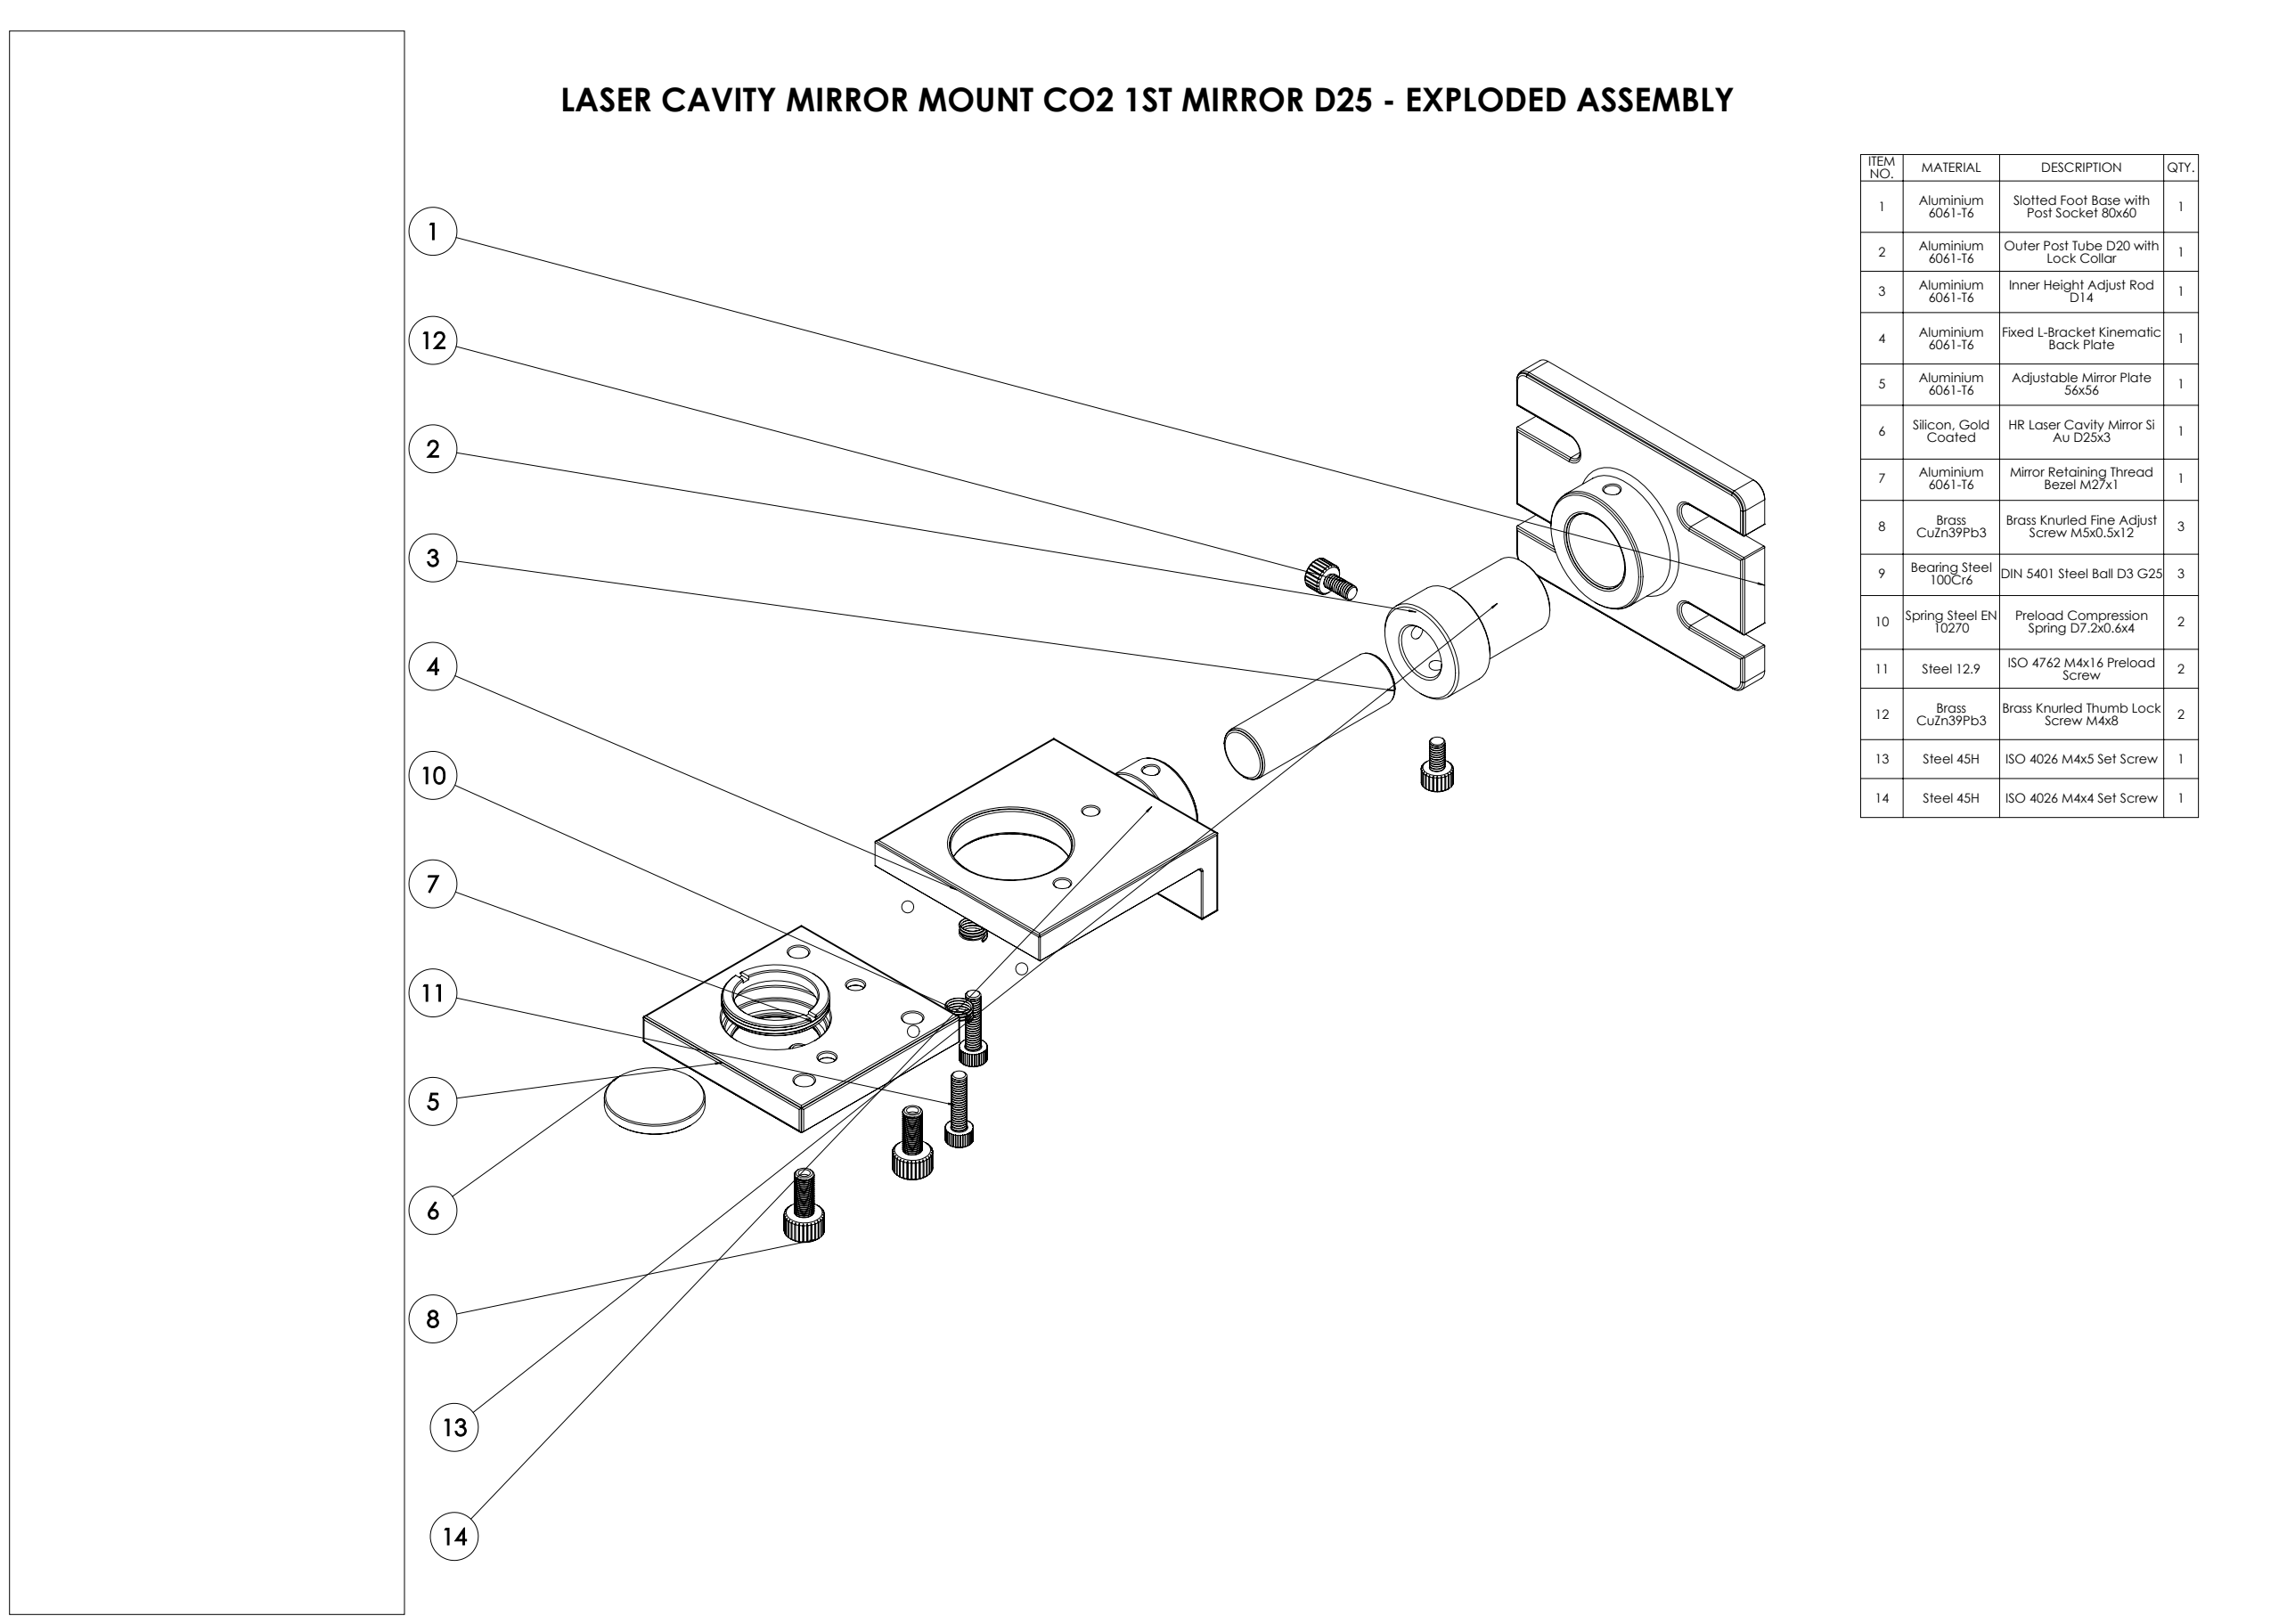
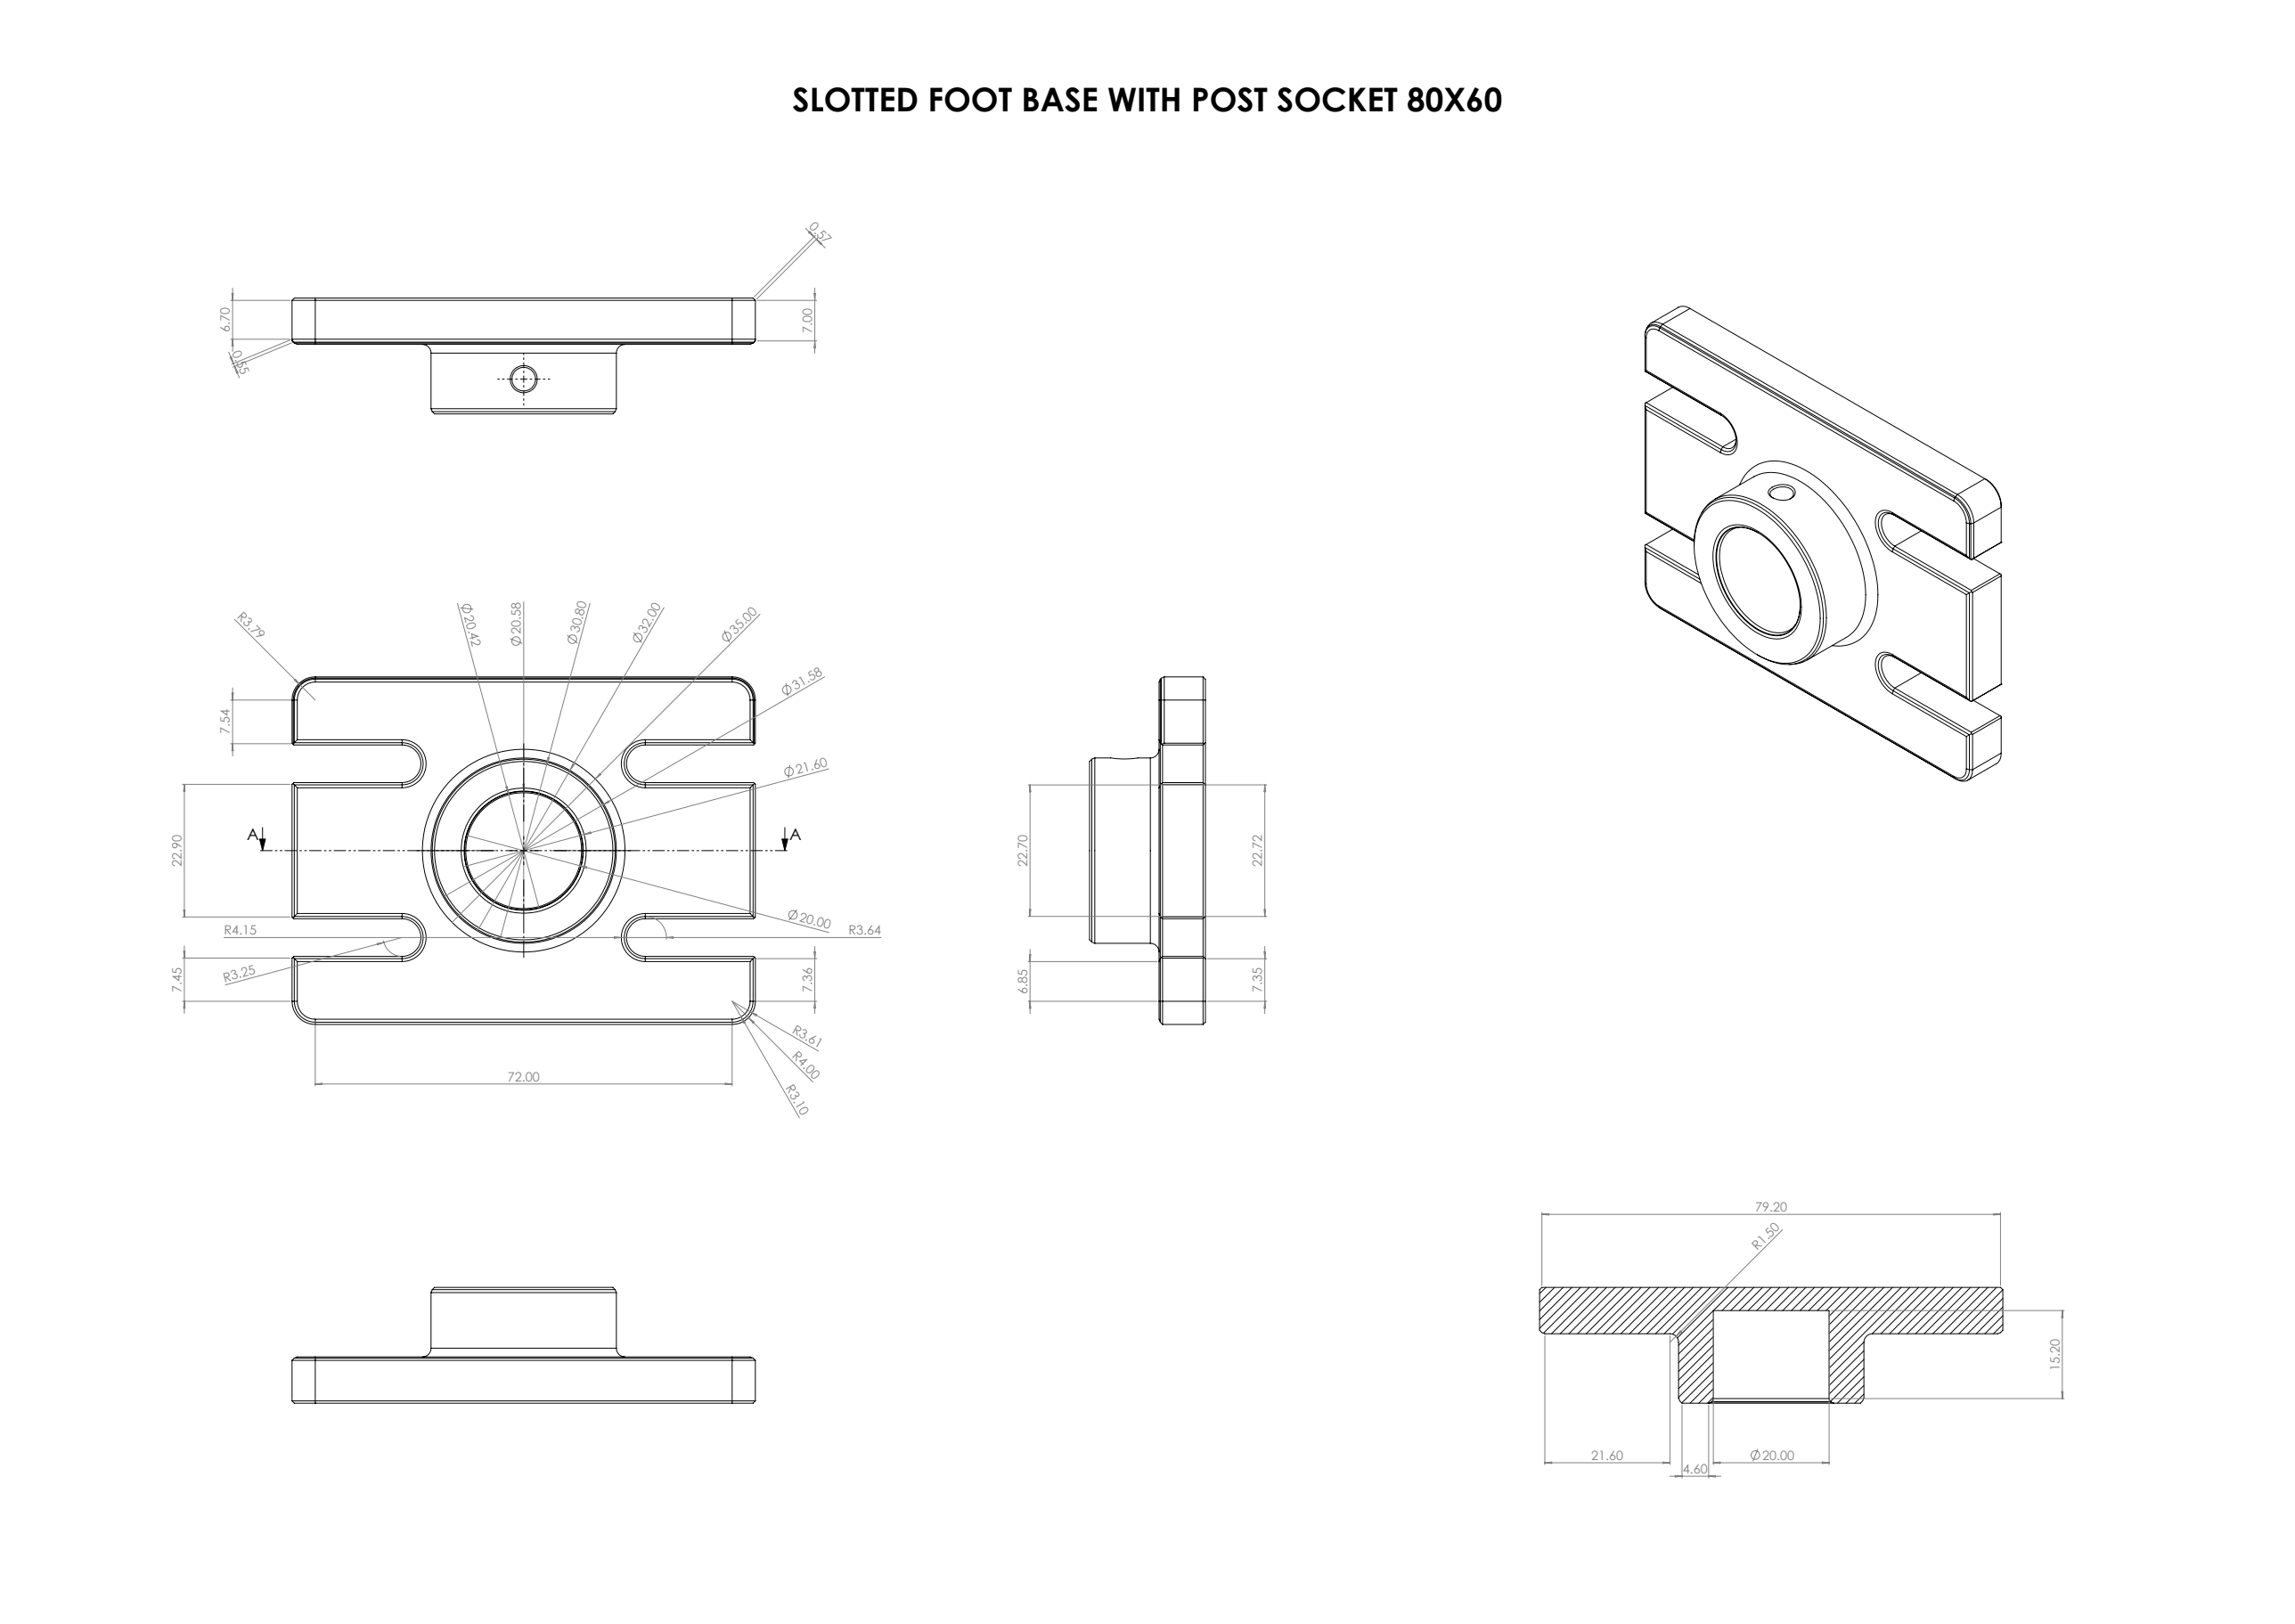
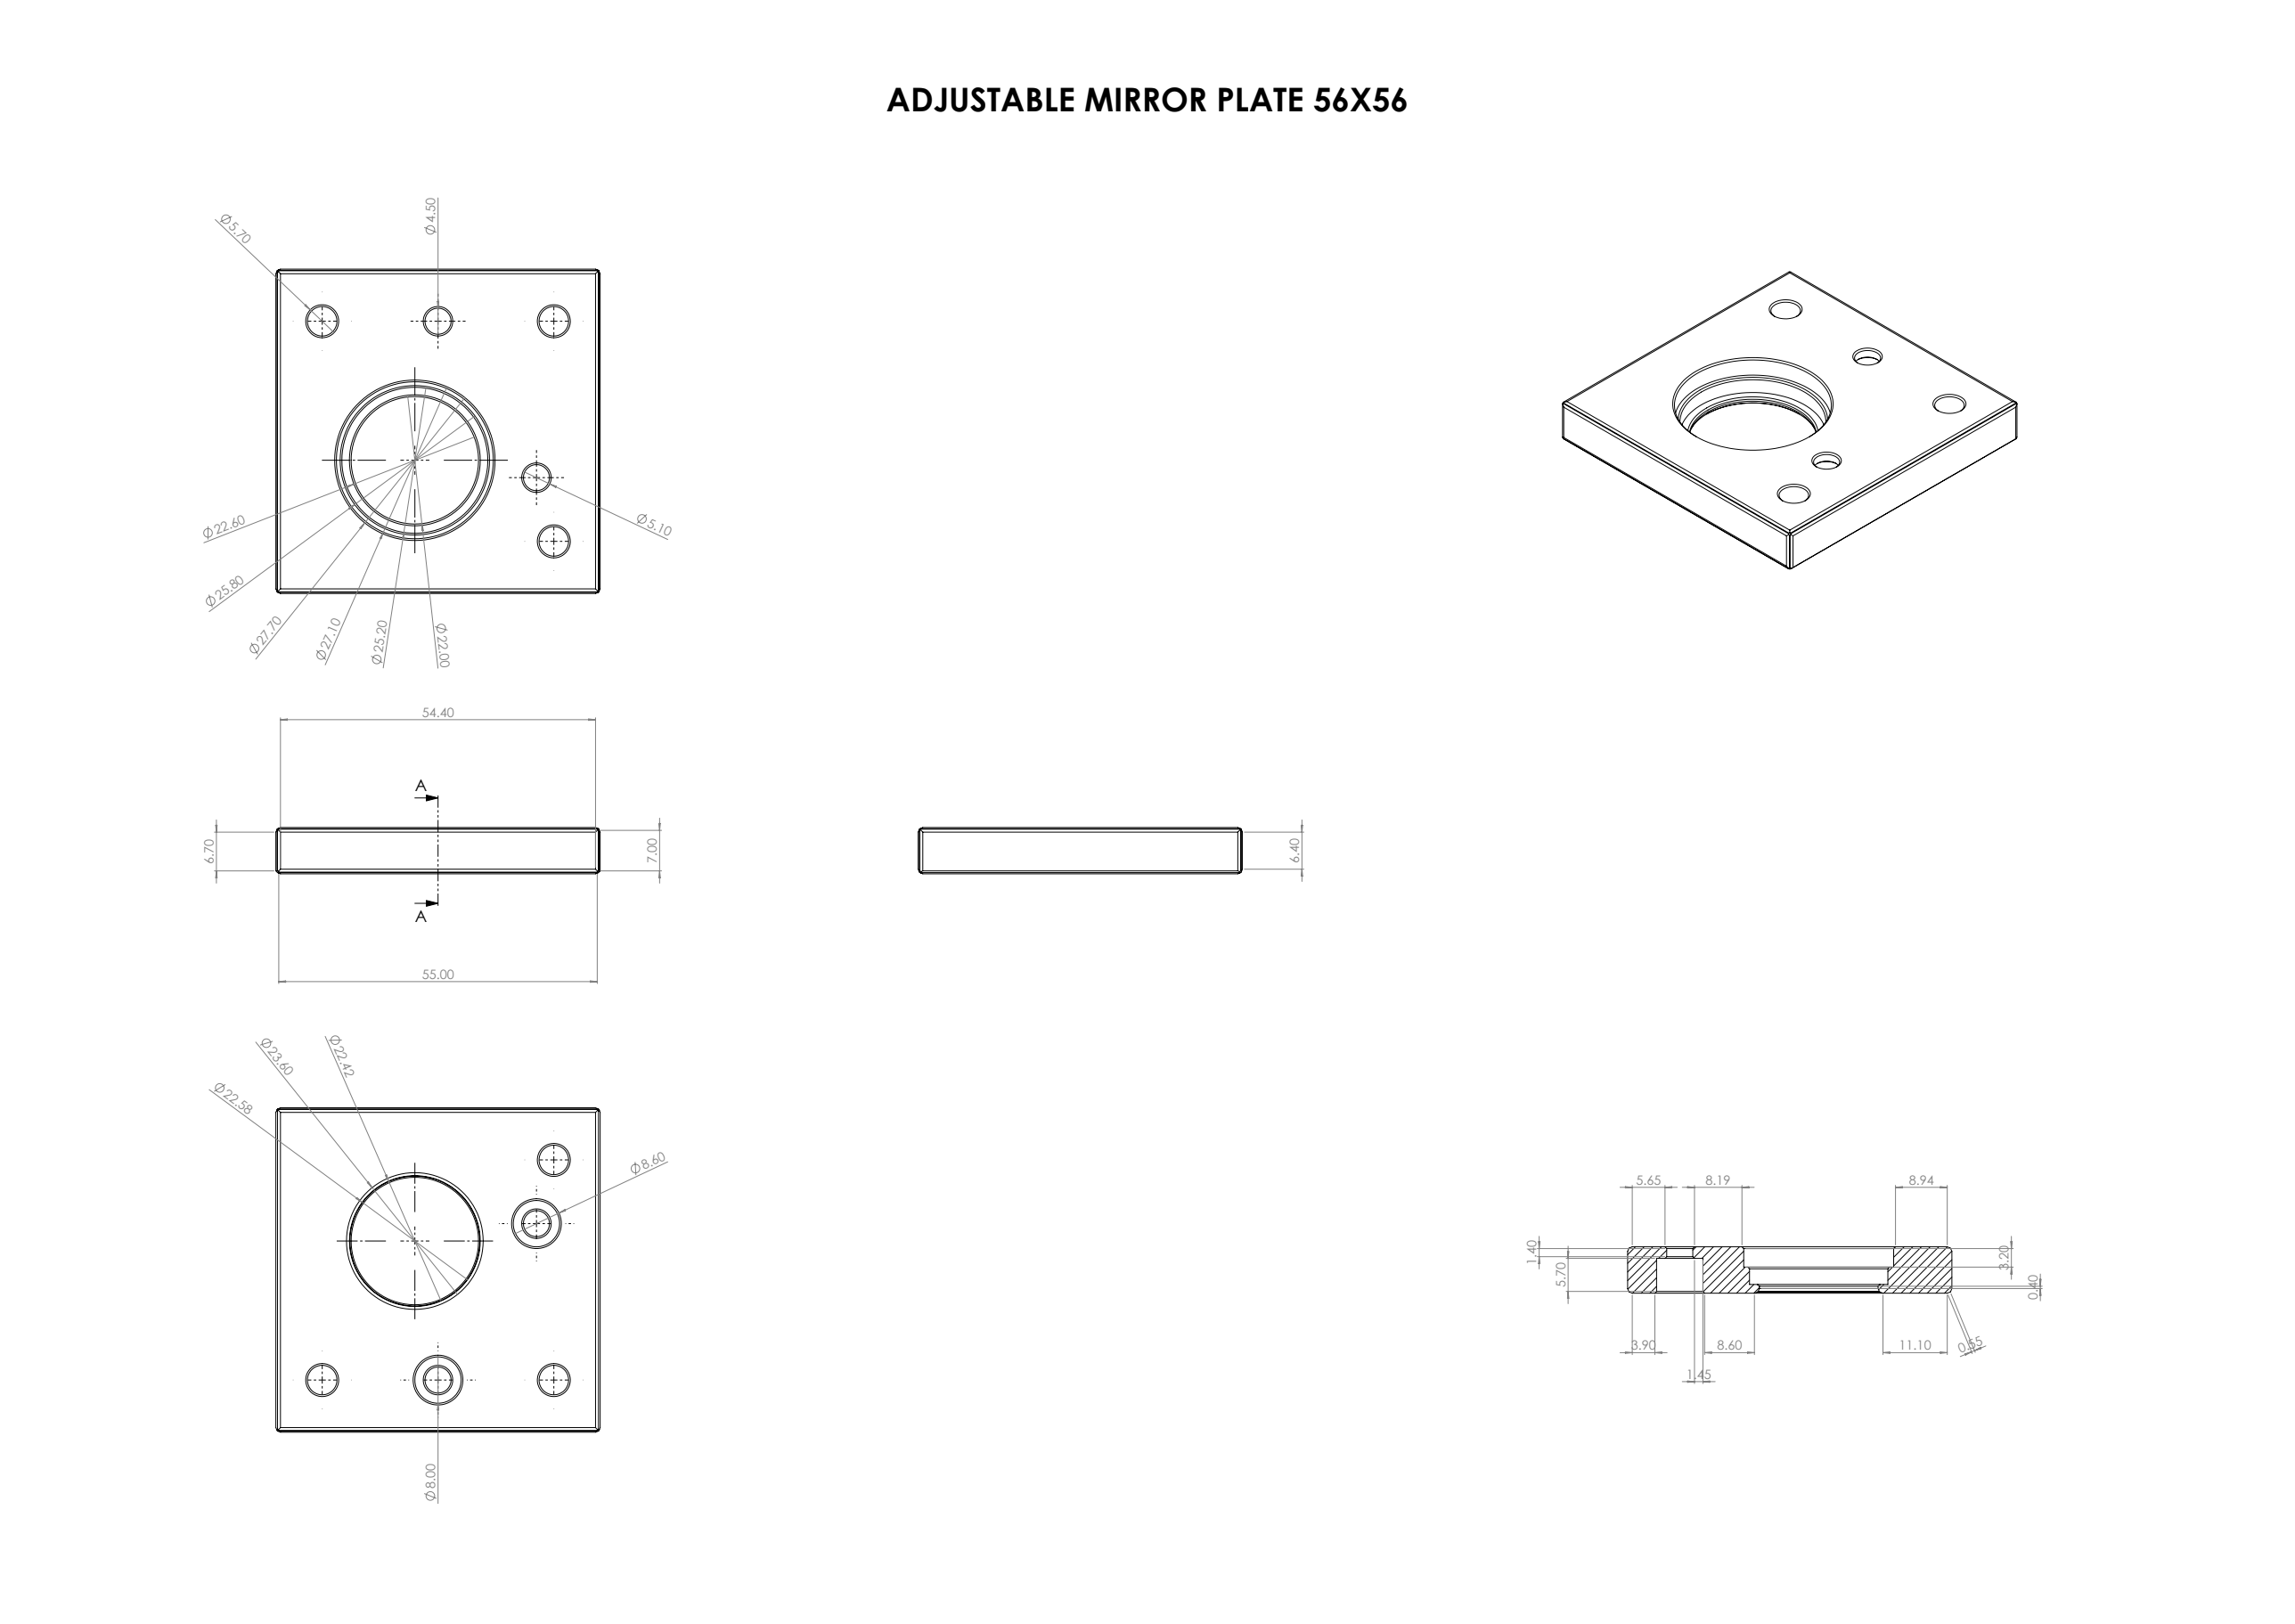
ISO-10303-21;
HEADER;
/* Generated by software containing ST-Developer
 * from STEP Tools, Inc. (www.steptools.com) 
 */

FILE_DESCRIPTION(
/* description */ (''),
/* implementation_level */ '2;1');

FILE_NAME(
/* name */ 
'MAS-303',
/* time_stamp */ '2026-10-20T10:06:23-07:00',
/* author */ (''),
/* organization */ (''),
/* preprocessor_version */ 'ST-DEVELOPER v20.2',
/* originating_system */ 'Autodesk Translation Framework v15.15.0.0',
/* authorisation */ '');

FILE_SCHEMA (('AUTOMOTIVE_DESIGN { 1 0 10303 214 3 1 1 }'));
ENDSEC;

DATA;
#10=MECHANICAL_DESIGN_GEOMETRIC_PRESENTATION_REPRESENTATION('',(#460,#461,
#462,#463,#464,#465,#466,#467,#468,#469,#470,#471,#472,#473),#38611);
#11=ITEM_DEFINED_TRANSFORMATION($,$,#16404,#17784);
#12=ITEM_DEFINED_TRANSFORMATION($,$,#16581,#17785);
#13=ITEM_DEFINED_TRANSFORMATION($,$,#16625,#17786);
#14=ITEM_DEFINED_TRANSFORMATION($,$,#16649,#17787);
#15=ITEM_DEFINED_TRANSFORMATION($,$,#16774,#17788);
#16=ITEM_DEFINED_TRANSFORMATION($,$,#16784,#17789);
#17=ITEM_DEFINED_TRANSFORMATION($,$,#17098,#17790);
#18=ITEM_DEFINED_TRANSFORMATION($,$,#17324,#17791);
#19=ITEM_DEFINED_TRANSFORMATION($,$,#17327,#17792);
#20=ITEM_DEFINED_TRANSFORMATION($,$,#17332,#17793);
#21=ITEM_DEFINED_TRANSFORMATION($,$,#17623,#17794);
#22=ITEM_DEFINED_TRANSFORMATION($,$,#16834,#17795);
#23=ITEM_DEFINED_TRANSFORMATION($,$,#16909,#17796);
#24=ITEM_DEFINED_TRANSFORMATION($,$,#16983,#17797);
#25=ITEM_DEFINED_TRANSFORMATION($,$,#17098,#17798);
#26=ITEM_DEFINED_TRANSFORMATION($,$,#17098,#17799);
#27=ITEM_DEFINED_TRANSFORMATION($,$,#17324,#17800);
#28=ITEM_DEFINED_TRANSFORMATION($,$,#17324,#17801);
#29=ITEM_DEFINED_TRANSFORMATION($,$,#17327,#17802);
#30=ITEM_DEFINED_TRANSFORMATION($,$,#17332,#17803);
#31=ITEM_DEFINED_TRANSFORMATION($,$,#17623,#17804);
#32=(
REPRESENTATION_RELATIONSHIP($,$,#38668,#38667)
REPRESENTATION_RELATIONSHIP_WITH_TRANSFORMATION(#11)
SHAPE_REPRESENTATION_RELATIONSHIP()
);
#33=(
REPRESENTATION_RELATIONSHIP($,$,#38669,#38667)
REPRESENTATION_RELATIONSHIP_WITH_TRANSFORMATION(#12)
SHAPE_REPRESENTATION_RELATIONSHIP()
);
#34=(
REPRESENTATION_RELATIONSHIP($,$,#38670,#38667)
REPRESENTATION_RELATIONSHIP_WITH_TRANSFORMATION(#13)
SHAPE_REPRESENTATION_RELATIONSHIP()
);
#35=(
REPRESENTATION_RELATIONSHIP($,$,#38671,#38667)
REPRESENTATION_RELATIONSHIP_WITH_TRANSFORMATION(#14)
SHAPE_REPRESENTATION_RELATIONSHIP()
);
#36=(
REPRESENTATION_RELATIONSHIP($,$,#38672,#38667)
REPRESENTATION_RELATIONSHIP_WITH_TRANSFORMATION(#15)
SHAPE_REPRESENTATION_RELATIONSHIP()
);
#37=(
REPRESENTATION_RELATIONSHIP($,$,#38673,#38667)
REPRESENTATION_RELATIONSHIP_WITH_TRANSFORMATION(#16)
SHAPE_REPRESENTATION_RELATIONSHIP()
);
#38=(
REPRESENTATION_RELATIONSHIP($,$,#38677,#38667)
REPRESENTATION_RELATIONSHIP_WITH_TRANSFORMATION(#17)
SHAPE_REPRESENTATION_RELATIONSHIP()
);
#39=(
REPRESENTATION_RELATIONSHIP($,$,#38678,#38667)
REPRESENTATION_RELATIONSHIP_WITH_TRANSFORMATION(#18)
SHAPE_REPRESENTATION_RELATIONSHIP()
);
#40=(
REPRESENTATION_RELATIONSHIP($,$,#38679,#38667)
REPRESENTATION_RELATIONSHIP_WITH_TRANSFORMATION(#19)
SHAPE_REPRESENTATION_RELATIONSHIP()
);
#41=(
REPRESENTATION_RELATIONSHIP($,$,#38680,#38667)
REPRESENTATION_RELATIONSHIP_WITH_TRANSFORMATION(#20)
SHAPE_REPRESENTATION_RELATIONSHIP()
);
#42=(
REPRESENTATION_RELATIONSHIP($,$,#38681,#38667)
REPRESENTATION_RELATIONSHIP_WITH_TRANSFORMATION(#21)
SHAPE_REPRESENTATION_RELATIONSHIP()
);
#43=(
REPRESENTATION_RELATIONSHIP($,$,#38674,#38667)
REPRESENTATION_RELATIONSHIP_WITH_TRANSFORMATION(#22)
SHAPE_REPRESENTATION_RELATIONSHIP()
);
#44=(
REPRESENTATION_RELATIONSHIP($,$,#38675,#38667)
REPRESENTATION_RELATIONSHIP_WITH_TRANSFORMATION(#23)
SHAPE_REPRESENTATION_RELATIONSHIP()
);
#45=(
REPRESENTATION_RELATIONSHIP($,$,#38676,#38667)
REPRESENTATION_RELATIONSHIP_WITH_TRANSFORMATION(#24)
SHAPE_REPRESENTATION_RELATIONSHIP()
);
#46=(
REPRESENTATION_RELATIONSHIP($,$,#38677,#38667)
REPRESENTATION_RELATIONSHIP_WITH_TRANSFORMATION(#25)
SHAPE_REPRESENTATION_RELATIONSHIP()
);
#47=(
REPRESENTATION_RELATIONSHIP($,$,#38677,#38667)
REPRESENTATION_RELATIONSHIP_WITH_TRANSFORMATION(#26)
SHAPE_REPRESENTATION_RELATIONSHIP()
);
#48=(
REPRESENTATION_RELATIONSHIP($,$,#38678,#38667)
REPRESENTATION_RELATIONSHIP_WITH_TRANSFORMATION(#27)
SHAPE_REPRESENTATION_RELATIONSHIP()
);
#49=(
REPRESENTATION_RELATIONSHIP($,$,#38678,#38667)
REPRESENTATION_RELATIONSHIP_WITH_TRANSFORMATION(#28)
SHAPE_REPRESENTATION_RELATIONSHIP()
);
#50=(
REPRESENTATION_RELATIONSHIP($,$,#38679,#38667)
REPRESENTATION_RELATIONSHIP_WITH_TRANSFORMATION(#29)
SHAPE_REPRESENTATION_RELATIONSHIP()
);
#51=(
REPRESENTATION_RELATIONSHIP($,$,#38680,#38667)
REPRESENTATION_RELATIONSHIP_WITH_TRANSFORMATION(#30)
SHAPE_REPRESENTATION_RELATIONSHIP()
);
#52=(
REPRESENTATION_RELATIONSHIP($,$,#38681,#38667)
REPRESENTATION_RELATIONSHIP_WITH_TRANSFORMATION(#31)
SHAPE_REPRESENTATION_RELATIONSHIP()
);
#53=CONTEXT_DEPENDENT_SHAPE_REPRESENTATION(#32,#38646);
#54=CONTEXT_DEPENDENT_SHAPE_REPRESENTATION(#33,#38647);
#55=CONTEXT_DEPENDENT_SHAPE_REPRESENTATION(#34,#38648);
#56=CONTEXT_DEPENDENT_SHAPE_REPRESENTATION(#35,#38649);
#57=CONTEXT_DEPENDENT_SHAPE_REPRESENTATION(#36,#38650);
#58=CONTEXT_DEPENDENT_SHAPE_REPRESENTATION(#37,#38651);
#59=CONTEXT_DEPENDENT_SHAPE_REPRESENTATION(#38,#38652);
#60=CONTEXT_DEPENDENT_SHAPE_REPRESENTATION(#39,#38653);
#61=CONTEXT_DEPENDENT_SHAPE_REPRESENTATION(#40,#38654);
#62=CONTEXT_DEPENDENT_SHAPE_REPRESENTATION(#41,#38655);
#63=CONTEXT_DEPENDENT_SHAPE_REPRESENTATION(#42,#38656);
#64=CONTEXT_DEPENDENT_SHAPE_REPRESENTATION(#43,#38657);
#65=CONTEXT_DEPENDENT_SHAPE_REPRESENTATION(#44,#38658);
#66=CONTEXT_DEPENDENT_SHAPE_REPRESENTATION(#45,#38659);
#67=CONTEXT_DEPENDENT_SHAPE_REPRESENTATION(#46,#38660);
#68=CONTEXT_DEPENDENT_SHAPE_REPRESENTATION(#47,#38661);
#69=CONTEXT_DEPENDENT_SHAPE_REPRESENTATION(#48,#38662);
#70=CONTEXT_DEPENDENT_SHAPE_REPRESENTATION(#49,#38663);
#71=CONTEXT_DEPENDENT_SHAPE_REPRESENTATION(#50,#38664);
#72=CONTEXT_DEPENDENT_SHAPE_REPRESENTATION(#51,#38665);
#73=CONTEXT_DEPENDENT_SHAPE_REPRESENTATION(#52,#38666);
#74=NEXT_ASSEMBLY_USAGE_OCCURRENCE(
'01_Slotted_Foot_Base_with_Post_Socket_80x60:1',
'01_Slotted_Foot_Base_with_Post_Socket_80x60:1',
'01_Slotted_Foot_Base_with_Post_Socket_80x60:1',#38683,#38684,
'01_Slotted_Foot_Base_with_Post_Socket_80x60:1');
#75=NEXT_ASSEMBLY_USAGE_OCCURRENCE(
'02_Outer_Post_Tube_D20_with_Lock_Collar:1',
'02_Outer_Post_Tube_D20_with_Lock_Collar:1',
'02_Outer_Post_Tube_D20_with_Lock_Collar:1',#38683,#38685,
'02_Outer_Post_Tube_D20_with_Lock_Collar:1');
#76=NEXT_ASSEMBLY_USAGE_OCCURRENCE('03_Inner_Height_Adjust_Rod_D14:1',
'03_Inner_Height_Adjust_Rod_D14:1','03_Inner_Height_Adjust_Rod_D14:1',#38683,
#38686,'03_Inner_Height_Adjust_Rod_D14:1');
#77=NEXT_ASSEMBLY_USAGE_OCCURRENCE('05_Adjustable_Mirror_Plate_56x56:1',
'05_Adjustable_Mirror_Plate_56x56:1',
'05_Adjustable_Mirror_Plate_56x56:1',#38683,#38687,
'05_Adjustable_Mirror_Plate_56x56:1');
#78=NEXT_ASSEMBLY_USAGE_OCCURRENCE(
'06_HR_Laser_Cavity_Mirror_Si_Au_D25x3:1',
'06_HR_Laser_Cavity_Mirror_Si_Au_D25x3:1',
'06_HR_Laser_Cavity_Mirror_Si_Au_D25x3:1',#38683,#38688,
'06_HR_Laser_Cavity_Mirror_Si_Au_D25x3:1');
#79=NEXT_ASSEMBLY_USAGE_OCCURRENCE(
'07_Mirror_Retaining_Thread_Bezel_M27x1:1',
'07_Mirror_Retaining_Thread_Bezel_M27x1:1',
'07_Mirror_Retaining_Thread_Bezel_M27x1:1',#38683,#38689,
'07_Mirror_Retaining_Thread_Bezel_M27x1:1');
#80=NEXT_ASSEMBLY_USAGE_OCCURRENCE(
'08_Brass_Knurled_Fine_Adjust_Screw_M5x0.5x12:1',
'08_Brass_Knurled_Fine_Adjust_Screw_M5x0.5x12:1',
'08_Brass_Knurled_Fine_Adjust_Screw_M5x0.5x12:1',#38683,#38693,
'08_Brass_Knurled_Fine_Adjust_Screw_M5x0.5x12:1');
#81=NEXT_ASSEMBLY_USAGE_OCCURRENCE('09_DIN_5401_Steel_Ball_D3_G25:1',
'09_DIN_5401_Steel_Ball_D3_G25:1','09_DIN_5401_Steel_Ball_D3_G25:1',#38683,
#38694,'09_DIN_5401_Steel_Ball_D3_G25:1');
#82=NEXT_ASSEMBLY_USAGE_OCCURRENCE(
'10_Preload_Compression_Spring_D7.2x0.6x4:1',
'10_Preload_Compression_Spring_D7.2x0.6x4:1',
'10_Preload_Compression_Spring_D7.2x0.6x4:1',#38683,#38695,
'10_Preload_Compression_Spring_D7.2x0.6x4:1');
#83=NEXT_ASSEMBLY_USAGE_OCCURRENCE('11_ISO_4762_M4x16_Preload_Screw:1',
'11_ISO_4762_M4x16_Preload_Screw:1','11_ISO_4762_M4x16_Preload_Screw:1',
#38683,#38696,'11_ISO_4762_M4x16_Preload_Screw:1');
#84=NEXT_ASSEMBLY_USAGE_OCCURRENCE(
'12_Brass_Knurled_Thumb_Lock_Screw_M4x8:1',
'12_Brass_Knurled_Thumb_Lock_Screw_M4x8:1',
'12_Brass_Knurled_Thumb_Lock_Screw_M4x8:1',#38683,#38697,
'12_Brass_Knurled_Thumb_Lock_Screw_M4x8:1');
#85=NEXT_ASSEMBLY_USAGE_OCCURRENCE('13_ISO_4026_M4x5_Set_Screw:1',
'13_ISO_4026_M4x5_Set_Screw:1','13_ISO_4026_M4x5_Set_Screw:1',#38683,#38690,
'13_ISO_4026_M4x5_Set_Screw:1');
#86=NEXT_ASSEMBLY_USAGE_OCCURRENCE('14_ISO_4026_M4x4_Set_Screw:1',
'14_ISO_4026_M4x4_Set_Screw:1','14_ISO_4026_M4x4_Set_Screw:1',#38683,#38691,
'14_ISO_4026_M4x4_Set_Screw:1');
#87=NEXT_ASSEMBLY_USAGE_OCCURRENCE(
'04_Fixed_L-Bracket_Kinematic_Back_Plate:1',
'04_Fixed_L-Bracket_Kinematic_Back_Plate:1',
'04_Fixed_L-Bracket_Kinematic_Back_Plate:1',#38683,#38692,
'04_Fixed_L-Bracket_Kinematic_Back_Plate:1');
#88=NEXT_ASSEMBLY_USAGE_OCCURRENCE(
'08_Brass_Knurled_Fine_Adjust_Screw_M5x0.5x12:2',
'08_Brass_Knurled_Fine_Adjust_Screw_M5x0.5x12:2',
'08_Brass_Knurled_Fine_Adjust_Screw_M5x0.5x12:2',#38683,#38693,
'08_Brass_Knurled_Fine_Adjust_Screw_M5x0.5x12:2');
#89=NEXT_ASSEMBLY_USAGE_OCCURRENCE(
'08_Brass_Knurled_Fine_Adjust_Screw_M5x0.5x12:3',
'08_Brass_Knurled_Fine_Adjust_Screw_M5x0.5x12:3',
'08_Brass_Knurled_Fine_Adjust_Screw_M5x0.5x12:3',#38683,#38693,
'08_Brass_Knurled_Fine_Adjust_Screw_M5x0.5x12:3');
#90=NEXT_ASSEMBLY_USAGE_OCCURRENCE('09_DIN_5401_Steel_Ball_D3_G25:2',
'09_DIN_5401_Steel_Ball_D3_G25:2','09_DIN_5401_Steel_Ball_D3_G25:2',#38683,
#38694,'09_DIN_5401_Steel_Ball_D3_G25:2');
#91=NEXT_ASSEMBLY_USAGE_OCCURRENCE('09_DIN_5401_Steel_Ball_D3_G25:3',
'09_DIN_5401_Steel_Ball_D3_G25:3','09_DIN_5401_Steel_Ball_D3_G25:3',#38683,
#38694,'09_DIN_5401_Steel_Ball_D3_G25:3');
#92=NEXT_ASSEMBLY_USAGE_OCCURRENCE(
'10_Preload_Compression_Spring_D7.2x0.6x4:2',
'10_Preload_Compression_Spring_D7.2x0.6x4:2',
'10_Preload_Compression_Spring_D7.2x0.6x4:2',#38683,#38695,
'10_Preload_Compression_Spring_D7.2x0.6x4:2');
#93=NEXT_ASSEMBLY_USAGE_OCCURRENCE('11_ISO_4762_M4x16_Preload_Screw:2',
'11_ISO_4762_M4x16_Preload_Screw:2','11_ISO_4762_M4x16_Preload_Screw:2',
#38683,#38696,'11_ISO_4762_M4x16_Preload_Screw:2');
#94=NEXT_ASSEMBLY_USAGE_OCCURRENCE(
'12_Brass_Knurled_Thumb_Lock_Screw_M4x8:2',
'12_Brass_Knurled_Thumb_Lock_Screw_M4x8:2',
'12_Brass_Knurled_Thumb_Lock_Screw_M4x8:2',#38683,#38697,
'12_Brass_Knurled_Thumb_Lock_Screw_M4x8:2');
#95=SPHERICAL_SURFACE('',#17325,0.15);
#96=ELLIPSE('',#16996,1.69705627484771,1.2);
#97=ELLIPSE('',#16998,1.69705627484771,1.2);
#98=(
BOUNDED_CURVE()
B_SPLINE_CURVE(2,(#24495,#24496,#24497),.UNSPECIFIED.,.F.,.F.)
B_SPLINE_CURVE_WITH_KNOTS((3,3),(0.,0.048540461555457),.UNSPECIFIED.)
CURVE()
GEOMETRIC_REPRESENTATION_ITEM()
RATIONAL_B_SPLINE_CURVE((1.,1.0000974490119,1.00002789674321))
REPRESENTATION_ITEM('')
);
#99=(
BOUNDED_CURVE()
B_SPLINE_CURVE(2,(#24501,#24502,#24503),.UNSPECIFIED.,.F.,.F.)
B_SPLINE_CURVE_WITH_KNOTS((3,3),(0.,0.0425206671334367),.UNSPECIFIED.)
CURVE()
GEOMETRIC_REPRESENTATION_ITEM()
RATIONAL_B_SPLINE_CURVE((1.,1.00010008479633,1.))
REPRESENTATION_ITEM('')
);
#100=(
BOUNDED_CURVE()
B_SPLINE_CURVE(2,(#24513,#24514,#24515),.UNSPECIFIED.,.F.,.F.)
B_SPLINE_CURVE_WITH_KNOTS((3,3),(0.,0.0425206671334366),.UNSPECIFIED.)
CURVE()
GEOMETRIC_REPRESENTATION_ITEM()
RATIONAL_B_SPLINE_CURVE((1.,1.00010008445539,1.))
REPRESENTATION_ITEM('')
);
#101=(
BOUNDED_CURVE()
B_SPLINE_CURVE(2,(#24518,#24519,#24520),.UNSPECIFIED.,.F.,.F.)
B_SPLINE_CURVE_WITH_KNOTS((3,3),(0.00810844555795414,0.0566489071109945),
 .UNSPECIFIED.)
CURVE()
GEOMETRIC_REPRESENTATION_ITEM()
RATIONAL_B_SPLINE_CURVE((1.00002789660287,1.00009744852162,1.))
REPRESENTATION_ITEM('')
);
#102=(
BOUNDED_CURVE()
B_SPLINE_CURVE(2,(#24534,#24535,#24536),.UNSPECIFIED.,.F.,.F.)
B_SPLINE_CURVE_WITH_KNOTS((3,3),(0.,0.0485404615530411),.UNSPECIFIED.)
CURVE()
GEOMETRIC_REPRESENTATION_ITEM()
RATIONAL_B_SPLINE_CURVE((1.,1.00009744852162,1.00002789660287))
REPRESENTATION_ITEM('')
);
#103=(
BOUNDED_CURVE()
B_SPLINE_CURVE(2,(#24540,#24541,#24542),.UNSPECIFIED.,.F.,.F.)
B_SPLINE_CURVE_WITH_KNOTS((3,3),(0.,0.0425206671334366),.UNSPECIFIED.)
CURVE()
GEOMETRIC_REPRESENTATION_ITEM()
RATIONAL_B_SPLINE_CURVE((1.,1.00010008445539,1.))
REPRESENTATION_ITEM('')
);
#104=(
BOUNDED_CURVE()
B_SPLINE_CURVE(2,(#24552,#24553,#24554),.UNSPECIFIED.,.F.,.F.)
B_SPLINE_CURVE_WITH_KNOTS((3,3),(0.,0.0425206671334367),.UNSPECIFIED.)
CURVE()
GEOMETRIC_REPRESENTATION_ITEM()
RATIONAL_B_SPLINE_CURVE((1.,1.00010008479633,1.))
REPRESENTATION_ITEM('')
);
#105=(
BOUNDED_CURVE()
B_SPLINE_CURVE(2,(#24557,#24558,#24559),.UNSPECIFIED.,.F.,.F.)
B_SPLINE_CURVE_WITH_KNOTS((3,3),(0.00810844555553747,0.0566489071109946),
 .UNSPECIFIED.)
CURVE()
GEOMETRIC_REPRESENTATION_ITEM()
RATIONAL_B_SPLINE_CURVE((1.00002789674321,1.0000974490119,1.))
REPRESENTATION_ITEM('')
);
#106=(
BOUNDED_CURVE()
B_SPLINE_CURVE(2,(#25662,#25663,#25664),.UNSPECIFIED.,.F.,.F.)
B_SPLINE_CURVE_WITH_KNOTS((3,3),(0.,0.00350597452849922),.UNSPECIFIED.)
CURVE()
GEOMETRIC_REPRESENTATION_ITEM()
RATIONAL_B_SPLINE_CURVE((1.,1.00010739978215,1.))
REPRESENTATION_ITEM('')
);
#107=(
BOUNDED_CURVE()
B_SPLINE_CURVE(2,(#25666,#25667,#25668),.UNSPECIFIED.,.F.,.F.)
B_SPLINE_CURVE_WITH_KNOTS((3,3),(0.,0.00350597452849927),.UNSPECIFIED.)
CURVE()
GEOMETRIC_REPRESENTATION_ITEM()
RATIONAL_B_SPLINE_CURVE((1.,1.00010739978482,1.))
REPRESENTATION_ITEM('')
);
#108=(
BOUNDED_CURVE()
B_SPLINE_CURVE(2,(#25671,#25672,#25673),.UNSPECIFIED.,.F.,.F.)
B_SPLINE_CURVE_WITH_KNOTS((3,3),(0.,0.0035059745284993),.UNSPECIFIED.)
CURVE()
GEOMETRIC_REPRESENTATION_ITEM()
RATIONAL_B_SPLINE_CURVE((1.,1.00010739978303,1.))
REPRESENTATION_ITEM('')
);
#109=(
BOUNDED_CURVE()
B_SPLINE_CURVE(2,(#25675,#25676,#25677),.UNSPECIFIED.,.F.,.F.)
B_SPLINE_CURVE_WITH_KNOTS((3,3),(0.,0.00350597452849931),.UNSPECIFIED.)
CURVE()
GEOMETRIC_REPRESENTATION_ITEM()
RATIONAL_B_SPLINE_CURVE((1.,1.00010739978394,1.))
REPRESENTATION_ITEM('')
);
#110=(
BOUNDED_CURVE()
B_SPLINE_CURVE(2,(#25680,#25681,#25682),.UNSPECIFIED.,.F.,.F.)
B_SPLINE_CURVE_WITH_KNOTS((3,3),(0.,0.0035059745284993),.UNSPECIFIED.)
CURVE()
GEOMETRIC_REPRESENTATION_ITEM()
RATIONAL_B_SPLINE_CURVE((1.,1.00010739978631,1.))
REPRESENTATION_ITEM('')
);
#111=(
BOUNDED_CURVE()
B_SPLINE_CURVE(2,(#25684,#25685,#25686),.UNSPECIFIED.,.F.,.F.)
B_SPLINE_CURVE_WITH_KNOTS((3,3),(0.,0.00350597452849929),.UNSPECIFIED.)
CURVE()
GEOMETRIC_REPRESENTATION_ITEM()
RATIONAL_B_SPLINE_CURVE((1.,1.00010739978645,1.))
REPRESENTATION_ITEM('')
);
#112=(
BOUNDED_CURVE()
B_SPLINE_CURVE(2,(#25689,#25690,#25691),.UNSPECIFIED.,.F.,.F.)
B_SPLINE_CURVE_WITH_KNOTS((3,3),(0.,0.0035059745284993),.UNSPECIFIED.)
CURVE()
GEOMETRIC_REPRESENTATION_ITEM()
RATIONAL_B_SPLINE_CURVE((1.,1.00010739979569,1.))
REPRESENTATION_ITEM('')
);
#113=(
BOUNDED_CURVE()
B_SPLINE_CURVE(2,(#25693,#25694,#25695),.UNSPECIFIED.,.F.,.F.)
B_SPLINE_CURVE_WITH_KNOTS((3,3),(0.,0.0035059745284993),.UNSPECIFIED.)
CURVE()
GEOMETRIC_REPRESENTATION_ITEM()
RATIONAL_B_SPLINE_CURVE((1.,1.00010739979698,1.))
REPRESENTATION_ITEM('')
);
#114=(
BOUNDED_CURVE()
B_SPLINE_CURVE(2,(#25698,#25699,#25700),.UNSPECIFIED.,.F.,.F.)
B_SPLINE_CURVE_WITH_KNOTS((3,3),(0.,0.00350597452849928),.UNSPECIFIED.)
CURVE()
GEOMETRIC_REPRESENTATION_ITEM()
RATIONAL_B_SPLINE_CURVE((1.,1.00010739978256,1.))
REPRESENTATION_ITEM('')
);
#115=(
BOUNDED_CURVE()
B_SPLINE_CURVE(2,(#25702,#25703,#25704),.UNSPECIFIED.,.F.,.F.)
B_SPLINE_CURVE_WITH_KNOTS((3,3),(0.,0.00350597452849928),.UNSPECIFIED.)
CURVE()
GEOMETRIC_REPRESENTATION_ITEM()
RATIONAL_B_SPLINE_CURVE((1.,1.00010739978752,1.))
REPRESENTATION_ITEM('')
);
#116=(
BOUNDED_CURVE()
B_SPLINE_CURVE(2,(#25707,#25708,#25709),.UNSPECIFIED.,.F.,.F.)
B_SPLINE_CURVE_WITH_KNOTS((3,3),(0.,0.0035059745284993),.UNSPECIFIED.)
CURVE()
GEOMETRIC_REPRESENTATION_ITEM()
RATIONAL_B_SPLINE_CURVE((1.,1.0001073997843,1.))
REPRESENTATION_ITEM('')
);
#117=(
BOUNDED_CURVE()
B_SPLINE_CURVE(2,(#25711,#25712,#25713),.UNSPECIFIED.,.F.,.F.)
B_SPLINE_CURVE_WITH_KNOTS((3,3),(0.,0.00350597452849929),.UNSPECIFIED.)
CURVE()
GEOMETRIC_REPRESENTATION_ITEM()
RATIONAL_B_SPLINE_CURVE((1.,1.00010739978875,1.))
REPRESENTATION_ITEM('')
);
#118=(
BOUNDED_CURVE()
B_SPLINE_CURVE(2,(#26703,#26704,#26705),.UNSPECIFIED.,.F.,.F.)
B_SPLINE_CURVE_WITH_KNOTS((3,3),(0.,0.00350597452849922),.UNSPECIFIED.)
CURVE()
GEOMETRIC_REPRESENTATION_ITEM()
RATIONAL_B_SPLINE_CURVE((1.,1.00010739978215,1.))
REPRESENTATION_ITEM('')
);
#119=(
BOUNDED_CURVE()
B_SPLINE_CURVE(2,(#26707,#26708,#26709),.UNSPECIFIED.,.F.,.F.)
B_SPLINE_CURVE_WITH_KNOTS((3,3),(0.,0.00350597452849927),.UNSPECIFIED.)
CURVE()
GEOMETRIC_REPRESENTATION_ITEM()
RATIONAL_B_SPLINE_CURVE((1.,1.00010739978482,1.))
REPRESENTATION_ITEM('')
);
#120=(
BOUNDED_CURVE()
B_SPLINE_CURVE(2,(#26712,#26713,#26714),.UNSPECIFIED.,.F.,.F.)
B_SPLINE_CURVE_WITH_KNOTS((3,3),(0.,0.0035059745284993),.UNSPECIFIED.)
CURVE()
GEOMETRIC_REPRESENTATION_ITEM()
RATIONAL_B_SPLINE_CURVE((1.,1.00010739978303,1.))
REPRESENTATION_ITEM('')
);
#121=(
BOUNDED_CURVE()
B_SPLINE_CURVE(2,(#26716,#26717,#26718),.UNSPECIFIED.,.F.,.F.)
B_SPLINE_CURVE_WITH_KNOTS((3,3),(0.,0.00350597452849931),.UNSPECIFIED.)
CURVE()
GEOMETRIC_REPRESENTATION_ITEM()
RATIONAL_B_SPLINE_CURVE((1.,1.00010739978394,1.))
REPRESENTATION_ITEM('')
);
#122=(
BOUNDED_CURVE()
B_SPLINE_CURVE(2,(#26721,#26722,#26723),.UNSPECIFIED.,.F.,.F.)
B_SPLINE_CURVE_WITH_KNOTS((3,3),(0.,0.0035059745284993),.UNSPECIFIED.)
CURVE()
GEOMETRIC_REPRESENTATION_ITEM()
RATIONAL_B_SPLINE_CURVE((1.,1.00010739978631,1.))
REPRESENTATION_ITEM('')
);
#123=(
BOUNDED_CURVE()
B_SPLINE_CURVE(2,(#26725,#26726,#26727),.UNSPECIFIED.,.F.,.F.)
B_SPLINE_CURVE_WITH_KNOTS((3,3),(0.,0.00350597452849929),.UNSPECIFIED.)
CURVE()
GEOMETRIC_REPRESENTATION_ITEM()
RATIONAL_B_SPLINE_CURVE((1.,1.00010739978645,1.))
REPRESENTATION_ITEM('')
);
#124=(
BOUNDED_CURVE()
B_SPLINE_CURVE(2,(#26730,#26731,#26732),.UNSPECIFIED.,.F.,.F.)
B_SPLINE_CURVE_WITH_KNOTS((3,3),(0.,0.0035059745284993),.UNSPECIFIED.)
CURVE()
GEOMETRIC_REPRESENTATION_ITEM()
RATIONAL_B_SPLINE_CURVE((1.,1.00010739979569,1.))
REPRESENTATION_ITEM('')
);
#125=(
BOUNDED_CURVE()
B_SPLINE_CURVE(2,(#26734,#26735,#26736),.UNSPECIFIED.,.F.,.F.)
B_SPLINE_CURVE_WITH_KNOTS((3,3),(0.,0.0035059745284993),.UNSPECIFIED.)
CURVE()
GEOMETRIC_REPRESENTATION_ITEM()
RATIONAL_B_SPLINE_CURVE((1.,1.00010739979698,1.))
REPRESENTATION_ITEM('')
);
#126=(
BOUNDED_CURVE()
B_SPLINE_CURVE(2,(#26739,#26740,#26741),.UNSPECIFIED.,.F.,.F.)
B_SPLINE_CURVE_WITH_KNOTS((3,3),(0.,0.00350597452849928),.UNSPECIFIED.)
CURVE()
GEOMETRIC_REPRESENTATION_ITEM()
RATIONAL_B_SPLINE_CURVE((1.,1.00010739978256,1.))
REPRESENTATION_ITEM('')
);
#127=(
BOUNDED_CURVE()
B_SPLINE_CURVE(2,(#26743,#26744,#26745),.UNSPECIFIED.,.F.,.F.)
B_SPLINE_CURVE_WITH_KNOTS((3,3),(0.,0.00350597452849928),.UNSPECIFIED.)
CURVE()
GEOMETRIC_REPRESENTATION_ITEM()
RATIONAL_B_SPLINE_CURVE((1.,1.00010739978752,1.))
REPRESENTATION_ITEM('')
);
#128=(
BOUNDED_CURVE()
B_SPLINE_CURVE(2,(#26748,#26749,#26750),.UNSPECIFIED.,.F.,.F.)
B_SPLINE_CURVE_WITH_KNOTS((3,3),(0.,0.0035059745284993),.UNSPECIFIED.)
CURVE()
GEOMETRIC_REPRESENTATION_ITEM()
RATIONAL_B_SPLINE_CURVE((1.,1.0001073997843,1.))
REPRESENTATION_ITEM('')
);
#129=(
BOUNDED_CURVE()
B_SPLINE_CURVE(2,(#26752,#26753,#26754),.UNSPECIFIED.,.F.,.F.)
B_SPLINE_CURVE_WITH_KNOTS((3,3),(0.,0.00350597452849929),.UNSPECIFIED.)
CURVE()
GEOMETRIC_REPRESENTATION_ITEM()
RATIONAL_B_SPLINE_CURVE((1.,1.00010739978875,1.))
REPRESENTATION_ITEM('')
);
#130=(
BOUNDED_CURVE()
B_SPLINE_CURVE(2,(#27130,#27131,#27132),.UNSPECIFIED.,.F.,.F.)
B_SPLINE_CURVE_WITH_KNOTS((3,3),(0.245470547469808,0.342025381879347),
 .UNSPECIFIED.)
CURVE()
GEOMETRIC_REPRESENTATION_ITEM()
RATIONAL_B_SPLINE_CURVE((1.,1.,1.))
REPRESENTATION_ITEM('')
);
#131=(
BOUNDED_CURVE()
B_SPLINE_CURVE(2,(#27135,#27136,#27137),.UNSPECIFIED.,.F.,.F.)
B_SPLINE_CURVE_WITH_KNOTS((3,3),(0.165943124807515,0.262497959217054),
 .UNSPECIFIED.)
CURVE()
GEOMETRIC_REPRESENTATION_ITEM()
RATIONAL_B_SPLINE_CURVE((1.,1.,1.))
REPRESENTATION_ITEM('')
);
#132=(
BOUNDED_CURVE()
B_SPLINE_CURVE(2,(#30814,#30815,#30816),.UNSPECIFIED.,.F.,.F.)
B_SPLINE_CURVE_WITH_KNOTS((3,3),(0.0467199500563867,0.0898699663113549),
 .UNSPECIFIED.)
CURVE()
GEOMETRIC_REPRESENTATION_ITEM()
RATIONAL_B_SPLINE_CURVE((1.00126937543075,1.00122087809448,1.))
REPRESENTATION_ITEM('')
);
#133=(
BOUNDED_CURVE()
B_SPLINE_CURVE(2,(#30820,#30821,#30822),.UNSPECIFIED.,.F.,.F.)
B_SPLINE_CURVE_WITH_KNOTS((3,3),(0.,0.0436887632258073),.UNSPECIFIED.)
CURVE()
GEOMETRIC_REPRESENTATION_ITEM()
RATIONAL_B_SPLINE_CURVE((1.,1.00100330533763,1.00083425612165))
REPRESENTATION_ITEM('')
);
#134=(
BOUNDED_CURVE()
B_SPLINE_CURVE(2,(#30826,#30827,#30828),.UNSPECIFIED.,.F.,.F.)
B_SPLINE_CURVE_WITH_KNOTS((3,3),(0.,0.0431500162549626),.UNSPECIFIED.)
CURVE()
GEOMETRIC_REPRESENTATION_ITEM()
RATIONAL_B_SPLINE_CURVE((1.,1.00122087809439,1.00126937543066))
REPRESENTATION_ITEM('')
);
#135=(
BOUNDED_CURVE()
B_SPLINE_CURVE(2,(#30831,#30832,#30833),.UNSPECIFIED.,.F.,.F.)
B_SPLINE_CURVE_WITH_KNOTS((3,3),(0.0310892451912064,0.0747780084169829),
 .UNSPECIFIED.)
CURVE()
GEOMETRIC_REPRESENTATION_ITEM()
RATIONAL_B_SPLINE_CURVE((1.00083425612186,1.00100330533789,1.))
REPRESENTATION_ITEM('')
);
#136=(
BOUNDED_CURVE()
B_SPLINE_CURVE(2,(#30837,#30838,#30839),.UNSPECIFIED.,.F.,.F.)
B_SPLINE_CURVE_WITH_KNOTS((3,3),(0.0467199500564158,0.089869966311355),
 .UNSPECIFIED.)
CURVE()
GEOMETRIC_REPRESENTATION_ITEM()
RATIONAL_B_SPLINE_CURVE((1.00126937543096,1.00122087809468,1.))
REPRESENTATION_ITEM('')
);
#137=(
BOUNDED_CURVE()
B_SPLINE_CURVE(2,(#30843,#30844,#30845),.UNSPECIFIED.,.F.,.F.)
B_SPLINE_CURVE_WITH_KNOTS((3,3),(0.,0.043688763225805),.UNSPECIFIED.)
CURVE()
GEOMETRIC_REPRESENTATION_ITEM()
RATIONAL_B_SPLINE_CURVE((1.,1.00100330533789,1.00083425612186))
REPRESENTATION_ITEM('')
);
#138=(
BOUNDED_CURVE()
B_SPLINE_CURVE(2,(#30849,#30850,#30851),.UNSPECIFIED.,.F.,.F.)
B_SPLINE_CURVE_WITH_KNOTS((3,3),(0.,0.0431500162549483),.UNSPECIFIED.)
CURVE()
GEOMETRIC_REPRESENTATION_ITEM()
RATIONAL_B_SPLINE_CURVE((1.,1.00122087809469,1.00126937543097))
REPRESENTATION_ITEM('')
);
#139=(
BOUNDED_CURVE()
B_SPLINE_CURVE(2,(#30854,#30855,#30856),.UNSPECIFIED.,.F.,.F.)
B_SPLINE_CURVE_WITH_KNOTS((3,3),(0.0310892451911987,0.0747780084169828),
 .UNSPECIFIED.)
CURVE()
GEOMETRIC_REPRESENTATION_ITEM()
RATIONAL_B_SPLINE_CURVE((1.00083425612161,1.00100330533758,1.))
REPRESENTATION_ITEM('')
);
#140=(
BOUNDED_CURVE()
B_SPLINE_CURVE(2,(#30860,#30861,#30862),.UNSPECIFIED.,.F.,.F.)
B_SPLINE_CURVE_WITH_KNOTS((3,3),(0.0467199500563958,0.089869966311355),
 .UNSPECIFIED.)
CURVE()
GEOMETRIC_REPRESENTATION_ITEM()
RATIONAL_B_SPLINE_CURVE((1.00126937543073,1.00122087809446,1.))
REPRESENTATION_ITEM('')
);
#141=(
BOUNDED_CURVE()
B_SPLINE_CURVE(2,(#30866,#30867,#30868),.UNSPECIFIED.,.F.,.F.)
B_SPLINE_CURVE_WITH_KNOTS((3,3),(0.,0.0436887632258068),.UNSPECIFIED.)
CURVE()
GEOMETRIC_REPRESENTATION_ITEM()
RATIONAL_B_SPLINE_CURVE((1.,1.0010033053375,1.00083425612154))
REPRESENTATION_ITEM('')
);
#142=(
BOUNDED_CURVE()
B_SPLINE_CURVE(2,(#30872,#30873,#30874),.UNSPECIFIED.,.F.,.F.)
B_SPLINE_CURVE_WITH_KNOTS((3,3),(0.,0.0431500162549413),.UNSPECIFIED.)
CURVE()
GEOMETRIC_REPRESENTATION_ITEM()
RATIONAL_B_SPLINE_CURVE((1.,1.00122087809486,1.00126937543114))
REPRESENTATION_ITEM('')
);
#143=(
BOUNDED_CURVE()
B_SPLINE_CURVE(2,(#30877,#30878,#30879),.UNSPECIFIED.,.F.,.F.)
B_SPLINE_CURVE_WITH_KNOTS((3,3),(0.0310892451911471,0.0747780084169828),
 .UNSPECIFIED.)
CURVE()
GEOMETRIC_REPRESENTATION_ITEM()
RATIONAL_B_SPLINE_CURVE((1.00083425612202,1.00100330533808,1.))
REPRESENTATION_ITEM('')
);
#144=(
BOUNDED_CURVE()
B_SPLINE_CURVE(2,(#30883,#30884,#30885),.UNSPECIFIED.,.F.,.F.)
B_SPLINE_CURVE_WITH_KNOTS((3,3),(0.046719950056407,0.089869966311355),
 .UNSPECIFIED.)
CURVE()
GEOMETRIC_REPRESENTATION_ITEM()
RATIONAL_B_SPLINE_CURVE((1.00126937543088,1.0012208780946,1.))
REPRESENTATION_ITEM('')
);
#145=(
BOUNDED_CURVE()
B_SPLINE_CURVE(2,(#30889,#30890,#30891),.UNSPECIFIED.,.F.,.F.)
B_SPLINE_CURVE_WITH_KNOTS((3,3),(0.,0.0436887632257949),.UNSPECIFIED.)
CURVE()
GEOMETRIC_REPRESENTATION_ITEM()
RATIONAL_B_SPLINE_CURVE((1.,1.00100330533737,1.00083425612143))
REPRESENTATION_ITEM('')
);
#146=(
BOUNDED_CURVE()
B_SPLINE_CURVE(2,(#30895,#30896,#30897),.UNSPECIFIED.,.F.,.F.)
B_SPLINE_CURVE_WITH_KNOTS((3,3),(0.,0.0431500162549611),.UNSPECIFIED.)
CURVE()
GEOMETRIC_REPRESENTATION_ITEM()
RATIONAL_B_SPLINE_CURVE((1.,1.00122087809444,1.00126937543071))
REPRESENTATION_ITEM('')
);
#147=(
BOUNDED_CURVE()
B_SPLINE_CURVE(2,(#30900,#30901,#30902),.UNSPECIFIED.,.F.,.F.)
B_SPLINE_CURVE_WITH_KNOTS((3,3),(0.0310892451911564,0.0747780084169829),
 .UNSPECIFIED.)
CURVE()
GEOMETRIC_REPRESENTATION_ITEM()
RATIONAL_B_SPLINE_CURVE((1.00083425612184,1.00100330533786,1.))
REPRESENTATION_ITEM('')
);
#148=(
BOUNDED_CURVE()
B_SPLINE_CURVE(2,(#30906,#30907,#30908),.UNSPECIFIED.,.F.,.F.)
B_SPLINE_CURVE_WITH_KNOTS((3,3),(0.0467199500563991,0.089869966311355),
 .UNSPECIFIED.)
CURVE()
GEOMETRIC_REPRESENTATION_ITEM()
RATIONAL_B_SPLINE_CURVE((1.00126937543067,1.0012208780944,1.))
REPRESENTATION_ITEM('')
);
#149=(
BOUNDED_CURVE()
B_SPLINE_CURVE(2,(#30912,#30913,#30914),.UNSPECIFIED.,.F.,.F.)
B_SPLINE_CURVE_WITH_KNOTS((3,3),(0.,0.0436887632258358),.UNSPECIFIED.)
CURVE()
GEOMETRIC_REPRESENTATION_ITEM()
RATIONAL_B_SPLINE_CURVE((1.,1.0010033053379,1.00083425612187))
REPRESENTATION_ITEM('')
);
#150=(
BOUNDED_CURVE()
B_SPLINE_CURVE(2,(#30918,#30919,#30920),.UNSPECIFIED.,.F.,.F.)
B_SPLINE_CURVE_WITH_KNOTS((3,3),(0.,0.0431500162549541),.UNSPECIFIED.)
CURVE()
GEOMETRIC_REPRESENTATION_ITEM()
RATIONAL_B_SPLINE_CURVE((1.,1.00122087809508,1.00126937543137))
REPRESENTATION_ITEM('')
);
#151=(
BOUNDED_CURVE()
B_SPLINE_CURVE(2,(#30923,#30924,#30925),.UNSPECIFIED.,.F.,.F.)
B_SPLINE_CURVE_WITH_KNOTS((3,3),(0.0310892451911811,0.0747780084169827),
 .UNSPECIFIED.)
CURVE()
GEOMETRIC_REPRESENTATION_ITEM()
RATIONAL_B_SPLINE_CURVE((1.0008342561216,1.00100330533758,1.))
REPRESENTATION_ITEM('')
);
#152=(
BOUNDED_CURVE()
B_SPLINE_CURVE(2,(#30929,#30930,#30931),.UNSPECIFIED.,.F.,.F.)
B_SPLINE_CURVE_WITH_KNOTS((3,3),(0.0467199500563772,0.0898699663113549),
 .UNSPECIFIED.)
CURVE()
GEOMETRIC_REPRESENTATION_ITEM()
RATIONAL_B_SPLINE_CURVE((1.00126937543116,1.00122087809487,1.))
REPRESENTATION_ITEM('')
);
#153=(
BOUNDED_CURVE()
B_SPLINE_CURVE(2,(#30935,#30936,#30937),.UNSPECIFIED.,.F.,.F.)
B_SPLINE_CURVE_WITH_KNOTS((3,3),(0.,0.0436887632258276),.UNSPECIFIED.)
CURVE()
GEOMETRIC_REPRESENTATION_ITEM()
RATIONAL_B_SPLINE_CURVE((1.,1.00100330533759,1.00083425612161))
REPRESENTATION_ITEM('')
);
#154=(
BOUNDED_CURVE()
B_SPLINE_CURVE(2,(#30941,#30942,#30943),.UNSPECIFIED.,.F.,.F.)
B_SPLINE_CURVE_WITH_KNOTS((3,3),(0.,0.0431500162549563),.UNSPECIFIED.)
CURVE()
GEOMETRIC_REPRESENTATION_ITEM()
RATIONAL_B_SPLINE_CURVE((1.,1.00122087809465,1.00126937543093))
REPRESENTATION_ITEM('')
);
#155=(
BOUNDED_CURVE()
B_SPLINE_CURVE(2,(#30946,#30947,#30948),.UNSPECIFIED.,.F.,.F.)
B_SPLINE_CURVE_WITH_KNOTS((3,3),(0.0310892451911613,0.0747780084169828),
 .UNSPECIFIED.)
CURVE()
GEOMETRIC_REPRESENTATION_ITEM()
RATIONAL_B_SPLINE_CURVE((1.00083425612131,1.00100330533723,1.))
REPRESENTATION_ITEM('')
);
#156=(
BOUNDED_CURVE()
B_SPLINE_CURVE(2,(#30952,#30953,#30954),.UNSPECIFIED.,.F.,.F.)
B_SPLINE_CURVE_WITH_KNOTS((3,3),(0.0467199500563946,0.0898699663113547),
 .UNSPECIFIED.)
CURVE()
GEOMETRIC_REPRESENTATION_ITEM()
RATIONAL_B_SPLINE_CURVE((1.00126937543097,1.00122087809469,1.))
REPRESENTATION_ITEM('')
);
#157=(
BOUNDED_CURVE()
B_SPLINE_CURVE(2,(#30958,#30959,#30960),.UNSPECIFIED.,.F.,.F.)
B_SPLINE_CURVE_WITH_KNOTS((3,3),(0.,0.0436887632258045),.UNSPECIFIED.)
CURVE()
GEOMETRIC_REPRESENTATION_ITEM()
RATIONAL_B_SPLINE_CURVE((1.,1.00100330533793,1.00083425612189))
REPRESENTATION_ITEM('')
);
#158=(
BOUNDED_CURVE()
B_SPLINE_CURVE(2,(#30964,#30965,#30966),.UNSPECIFIED.,.F.,.F.)
B_SPLINE_CURVE_WITH_KNOTS((3,3),(0.,0.0431500162549573),.UNSPECIFIED.)
CURVE()
GEOMETRIC_REPRESENTATION_ITEM()
RATIONAL_B_SPLINE_CURVE((1.,1.00122087809474,1.00126937543102))
REPRESENTATION_ITEM('')
);
#159=(
BOUNDED_CURVE()
B_SPLINE_CURVE(2,(#30969,#30970,#30971),.UNSPECIFIED.,.F.,.F.)
B_SPLINE_CURVE_WITH_KNOTS((3,3),(0.0310892451911831,0.074778008416983),
 .UNSPECIFIED.)
CURVE()
GEOMETRIC_REPRESENTATION_ITEM()
RATIONAL_B_SPLINE_CURVE((1.00083425612233,1.00100330533846,1.))
REPRESENTATION_ITEM('')
);
#160=(
BOUNDED_CURVE()
B_SPLINE_CURVE(2,(#30975,#30976,#30977),.UNSPECIFIED.,.F.,.F.)
B_SPLINE_CURVE_WITH_KNOTS((3,3),(0.0467199500564136,0.0898699663113549),
 .UNSPECIFIED.)
CURVE()
GEOMETRIC_REPRESENTATION_ITEM()
RATIONAL_B_SPLINE_CURVE((1.00126937543068,1.00122087809441,1.))
REPRESENTATION_ITEM('')
);
#161=(
BOUNDED_CURVE()
B_SPLINE_CURVE(2,(#30981,#30982,#30983),.UNSPECIFIED.,.F.,.F.)
B_SPLINE_CURVE_WITH_KNOTS((3,3),(0.,0.0436887632258141),.UNSPECIFIED.)
CURVE()
GEOMETRIC_REPRESENTATION_ITEM()
RATIONAL_B_SPLINE_CURVE((1.,1.00100330533752,1.00083425612155))
REPRESENTATION_ITEM('')
);
#162=(
BOUNDED_CURVE()
B_SPLINE_CURVE(2,(#30987,#30988,#30989),.UNSPECIFIED.,.F.,.F.)
B_SPLINE_CURVE_WITH_KNOTS((3,3),(0.,0.0431500162549441),.UNSPECIFIED.)
CURVE()
GEOMETRIC_REPRESENTATION_ITEM()
RATIONAL_B_SPLINE_CURVE((1.,1.00122087809436,1.00126937543063))
REPRESENTATION_ITEM('')
);
#163=(
BOUNDED_CURVE()
B_SPLINE_CURVE(2,(#30992,#30993,#30994),.UNSPECIFIED.,.F.,.F.)
B_SPLINE_CURVE_WITH_KNOTS((3,3),(0.0310892451911682,0.0747780084169828),
 .UNSPECIFIED.)
CURVE()
GEOMETRIC_REPRESENTATION_ITEM()
RATIONAL_B_SPLINE_CURVE((1.00083425612141,1.00100330533735,1.))
REPRESENTATION_ITEM('')
);
#164=(
BOUNDED_CURVE()
B_SPLINE_CURVE(2,(#30998,#30999,#31000),.UNSPECIFIED.,.F.,.F.)
B_SPLINE_CURVE_WITH_KNOTS((3,3),(0.0467199500564218,0.0898699663113548),
 .UNSPECIFIED.)
CURVE()
GEOMETRIC_REPRESENTATION_ITEM()
RATIONAL_B_SPLINE_CURVE((1.00126937543122,1.00122087809493,1.))
REPRESENTATION_ITEM('')
);
#165=(
BOUNDED_CURVE()
B_SPLINE_CURVE(2,(#31004,#31005,#31006),.UNSPECIFIED.,.F.,.F.)
B_SPLINE_CURVE_WITH_KNOTS((3,3),(0.,0.0436887632257843),.UNSPECIFIED.)
CURVE()
GEOMETRIC_REPRESENTATION_ITEM()
RATIONAL_B_SPLINE_CURVE((1.,1.00100330533799,1.00083425612195))
REPRESENTATION_ITEM('')
);
#166=(
BOUNDED_CURVE()
B_SPLINE_CURVE(2,(#31010,#31011,#31012),.UNSPECIFIED.,.F.,.F.)
B_SPLINE_CURVE_WITH_KNOTS((3,3),(0.,0.0431500162549522),.UNSPECIFIED.)
CURVE()
GEOMETRIC_REPRESENTATION_ITEM()
RATIONAL_B_SPLINE_CURVE((1.,1.00122087809455,1.00126937543082))
REPRESENTATION_ITEM('')
);
#167=(
BOUNDED_CURVE()
B_SPLINE_CURVE(2,(#31015,#31016,#31017),.UNSPECIFIED.,.F.,.F.)
B_SPLINE_CURVE_WITH_KNOTS((3,3),(0.0310892451912127,0.0747780084169828),
 .UNSPECIFIED.)
CURVE()
GEOMETRIC_REPRESENTATION_ITEM()
RATIONAL_B_SPLINE_CURVE((1.000834256122,1.00100330533806,1.))
REPRESENTATION_ITEM('')
);
#168=(
BOUNDED_CURVE()
B_SPLINE_CURVE(2,(#31021,#31022,#31023),.UNSPECIFIED.,.F.,.F.)
B_SPLINE_CURVE_WITH_KNOTS((3,3),(0.046719950056375,0.0898699663113549),
 .UNSPECIFIED.)
CURVE()
GEOMETRIC_REPRESENTATION_ITEM()
RATIONAL_B_SPLINE_CURVE((1.00126937543081,1.00122087809453,1.))
REPRESENTATION_ITEM('')
);
#169=(
BOUNDED_CURVE()
B_SPLINE_CURVE(2,(#31027,#31028,#31029),.UNSPECIFIED.,.F.,.F.)
B_SPLINE_CURVE_WITH_KNOTS((3,3),(0.,0.043688763225798),.UNSPECIFIED.)
CURVE()
GEOMETRIC_REPRESENTATION_ITEM()
RATIONAL_B_SPLINE_CURVE((1.,1.00100330533766,1.00083425612167))
REPRESENTATION_ITEM('')
);
#170=(
BOUNDED_CURVE()
B_SPLINE_CURVE(2,(#31033,#31034,#31035),.UNSPECIFIED.,.F.,.F.)
B_SPLINE_CURVE_WITH_KNOTS((3,3),(0.,0.0431500162549388),.UNSPECIFIED.)
CURVE()
GEOMETRIC_REPRESENTATION_ITEM()
RATIONAL_B_SPLINE_CURVE((1.,1.00122087809441,1.00126937543068))
REPRESENTATION_ITEM('')
);
#171=(
BOUNDED_CURVE()
B_SPLINE_CURVE(2,(#31038,#31039,#31040),.UNSPECIFIED.,.F.,.F.)
B_SPLINE_CURVE_WITH_KNOTS((3,3),(0.031089245191172,0.0747780084169828),
 .UNSPECIFIED.)
CURVE()
GEOMETRIC_REPRESENTATION_ITEM()
RATIONAL_B_SPLINE_CURVE((1.00083425612203,1.00100330533809,1.))
REPRESENTATION_ITEM('')
);
#172=(
BOUNDED_CURVE()
B_SPLINE_CURVE(2,(#31044,#31045,#31046),.UNSPECIFIED.,.F.,.F.)
B_SPLINE_CURVE_WITH_KNOTS((3,3),(0.0467199500564012,0.0898699663113549),
 .UNSPECIFIED.)
CURVE()
GEOMETRIC_REPRESENTATION_ITEM()
RATIONAL_B_SPLINE_CURVE((1.00126937543067,1.00122087809441,1.))
REPRESENTATION_ITEM('')
);
#173=(
BOUNDED_CURVE()
B_SPLINE_CURVE(2,(#31050,#31051,#31052),.UNSPECIFIED.,.F.,.F.)
B_SPLINE_CURVE_WITH_KNOTS((3,3),(0.,0.0436887632258383),.UNSPECIFIED.)
CURVE()
GEOMETRIC_REPRESENTATION_ITEM()
RATIONAL_B_SPLINE_CURVE((1.,1.00100330533736,1.00083425612142))
REPRESENTATION_ITEM('')
);
#174=(
BOUNDED_CURVE()
B_SPLINE_CURVE(2,(#31056,#31057,#31058),.UNSPECIFIED.,.F.,.F.)
B_SPLINE_CURVE_WITH_KNOTS((3,3),(0.,0.0431500162549534),.UNSPECIFIED.)
CURVE()
GEOMETRIC_REPRESENTATION_ITEM()
RATIONAL_B_SPLINE_CURVE((1.,1.00122087809426,1.00126937543052))
REPRESENTATION_ITEM('')
);
#175=(
BOUNDED_CURVE()
B_SPLINE_CURVE(2,(#31061,#31062,#31063),.UNSPECIFIED.,.F.,.F.)
B_SPLINE_CURVE_WITH_KNOTS((3,3),(0.0310892451911742,0.074778008416983),
 .UNSPECIFIED.)
CURVE()
GEOMETRIC_REPRESENTATION_ITEM()
RATIONAL_B_SPLINE_CURVE((1.00083425612157,1.00100330533753,1.))
REPRESENTATION_ITEM('')
);
#176=(
BOUNDED_CURVE()
B_SPLINE_CURVE(2,(#31067,#31068,#31069),.UNSPECIFIED.,.F.,.F.)
B_SPLINE_CURVE_WITH_KNOTS((3,3),(0.0467199500564228,0.0898699663113548),
 .UNSPECIFIED.)
CURVE()
GEOMETRIC_REPRESENTATION_ITEM()
RATIONAL_B_SPLINE_CURVE((1.00126937543075,1.00122087809448,1.))
REPRESENTATION_ITEM('')
);
#177=(
BOUNDED_CURVE()
B_SPLINE_CURVE(2,(#31073,#31074,#31075),.UNSPECIFIED.,.F.,.F.)
B_SPLINE_CURVE_WITH_KNOTS((3,3),(0.,0.0436887632258167),.UNSPECIFIED.)
CURVE()
GEOMETRIC_REPRESENTATION_ITEM()
RATIONAL_B_SPLINE_CURVE((1.,1.0010033053373,1.00083425612137))
REPRESENTATION_ITEM('')
);
#178=(
BOUNDED_CURVE()
B_SPLINE_CURVE(2,(#31079,#31080,#31081),.UNSPECIFIED.,.F.,.F.)
B_SPLINE_CURVE_WITH_KNOTS((3,3),(0.,0.0431500162549855),.UNSPECIFIED.)
CURVE()
GEOMETRIC_REPRESENTATION_ITEM()
RATIONAL_B_SPLINE_CURVE((1.,1.00122087809442,1.00126937543069))
REPRESENTATION_ITEM('')
);
#179=(
BOUNDED_CURVE()
B_SPLINE_CURVE(2,(#31084,#31085,#31086),.UNSPECIFIED.,.F.,.F.)
B_SPLINE_CURVE_WITH_KNOTS((3,3),(0.0310892451911962,0.0747780084169828),
 .UNSPECIFIED.)
CURVE()
GEOMETRIC_REPRESENTATION_ITEM()
RATIONAL_B_SPLINE_CURVE((1.00083425612222,1.00100330533831,1.))
REPRESENTATION_ITEM('')
);
#180=(
BOUNDED_CURVE()
B_SPLINE_CURVE(2,(#31090,#31091,#31092),.UNSPECIFIED.,.F.,.F.)
B_SPLINE_CURVE_WITH_KNOTS((3,3),(0.0467199500564075,0.0898699663113548),
 .UNSPECIFIED.)
CURVE()
GEOMETRIC_REPRESENTATION_ITEM()
RATIONAL_B_SPLINE_CURVE((1.00126937543101,1.00122087809473,1.))
REPRESENTATION_ITEM('')
);
#181=(
BOUNDED_CURVE()
B_SPLINE_CURVE(2,(#31096,#31097,#31098),.UNSPECIFIED.,.F.,.F.)
B_SPLINE_CURVE_WITH_KNOTS((3,3),(0.,0.0436887632257957),.UNSPECIFIED.)
CURVE()
GEOMETRIC_REPRESENTATION_ITEM()
RATIONAL_B_SPLINE_CURVE((1.,1.00100330533777,1.00083425612177))
REPRESENTATION_ITEM('')
);
#182=(
BOUNDED_CURVE()
B_SPLINE_CURVE(2,(#31102,#31103,#31104),.UNSPECIFIED.,.F.,.F.)
B_SPLINE_CURVE_WITH_KNOTS((3,3),(0.,0.0431500162549319),.UNSPECIFIED.)
CURVE()
GEOMETRIC_REPRESENTATION_ITEM()
RATIONAL_B_SPLINE_CURVE((1.,1.00122087809489,1.00126937543118))
REPRESENTATION_ITEM('')
);
#183=(
BOUNDED_CURVE()
B_SPLINE_CURVE(2,(#31107,#31108,#31109),.UNSPECIFIED.,.F.,.F.)
B_SPLINE_CURVE_WITH_KNOTS((3,3),(0.0310892451911674,0.0747780084169828),
 .UNSPECIFIED.)
CURVE()
GEOMETRIC_REPRESENTATION_ITEM()
RATIONAL_B_SPLINE_CURVE((1.00083425612107,1.00100330533693,1.))
REPRESENTATION_ITEM('')
);
#184=(
BOUNDED_CURVE()
B_SPLINE_CURVE(2,(#31113,#31114,#31115),.UNSPECIFIED.,.F.,.F.)
B_SPLINE_CURVE_WITH_KNOTS((3,3),(0.0467199500564182,0.0898699663113548),
 .UNSPECIFIED.)
CURVE()
GEOMETRIC_REPRESENTATION_ITEM()
RATIONAL_B_SPLINE_CURVE((1.00126937543111,1.00122087809482,1.))
REPRESENTATION_ITEM('')
);
#185=(
BOUNDED_CURVE()
B_SPLINE_CURVE(2,(#31119,#31120,#31121),.UNSPECIFIED.,.F.,.F.)
B_SPLINE_CURVE_WITH_KNOTS((3,3),(0.,0.0436887632258121),.UNSPECIFIED.)
CURVE()
GEOMETRIC_REPRESENTATION_ITEM()
RATIONAL_B_SPLINE_CURVE((1.,1.00100330533764,1.00083425612165))
REPRESENTATION_ITEM('')
);
#186=(
BOUNDED_CURVE()
B_SPLINE_CURVE(2,(#31125,#31126,#31127),.UNSPECIFIED.,.F.,.F.)
B_SPLINE_CURVE_WITH_KNOTS((3,3),(0.,0.0431500162549636),.UNSPECIFIED.)
CURVE()
GEOMETRIC_REPRESENTATION_ITEM()
RATIONAL_B_SPLINE_CURVE((1.,1.0012208780943,1.00126937543056))
REPRESENTATION_ITEM('')
);
#187=(
BOUNDED_CURVE()
B_SPLINE_CURVE(2,(#31130,#31131,#31132),.UNSPECIFIED.,.F.,.F.)
B_SPLINE_CURVE_WITH_KNOTS((3,3),(0.0310892451911629,0.0747780084169827),
 .UNSPECIFIED.)
CURVE()
GEOMETRIC_REPRESENTATION_ITEM()
RATIONAL_B_SPLINE_CURVE((1.00083425612137,1.0010033053373,1.))
REPRESENTATION_ITEM('')
);
#188=(
BOUNDED_CURVE()
B_SPLINE_CURVE(2,(#31136,#31137,#31138),.UNSPECIFIED.,.F.,.F.)
B_SPLINE_CURVE_WITH_KNOTS((3,3),(0.0467199500564021,0.0898699663113548),
 .UNSPECIFIED.)
CURVE()
GEOMETRIC_REPRESENTATION_ITEM()
RATIONAL_B_SPLINE_CURVE((1.00126937543099,1.00122087809471,1.))
REPRESENTATION_ITEM('')
);
#189=(
BOUNDED_CURVE()
B_SPLINE_CURVE(2,(#31142,#31143,#31144),.UNSPECIFIED.,.F.,.F.)
B_SPLINE_CURVE_WITH_KNOTS((3,3),(0.,0.0436887632258091),.UNSPECIFIED.)
CURVE()
GEOMETRIC_REPRESENTATION_ITEM()
RATIONAL_B_SPLINE_CURVE((1.,1.00100330533755,1.00083425612158))
REPRESENTATION_ITEM('')
);
#190=(
BOUNDED_CURVE()
B_SPLINE_CURVE(2,(#31148,#31149,#31150),.UNSPECIFIED.,.F.,.F.)
B_SPLINE_CURVE_WITH_KNOTS((3,3),(0.,0.0431500162549568),.UNSPECIFIED.)
CURVE()
GEOMETRIC_REPRESENTATION_ITEM()
RATIONAL_B_SPLINE_CURVE((1.,1.00122087809472,1.00126937543101))
REPRESENTATION_ITEM('')
);
#191=(
BOUNDED_CURVE()
B_SPLINE_CURVE(2,(#31153,#31154,#31155),.UNSPECIFIED.,.F.,.F.)
B_SPLINE_CURVE_WITH_KNOTS((3,3),(0.0310892451911866,0.0747780084169829),
 .UNSPECIFIED.)
CURVE()
GEOMETRIC_REPRESENTATION_ITEM()
RATIONAL_B_SPLINE_CURVE((1.0008342561218,1.00100330533782,1.))
REPRESENTATION_ITEM('')
);
#192=(
BOUNDED_CURVE()
B_SPLINE_CURVE(2,(#31159,#31160,#31161),.UNSPECIFIED.,.F.,.F.)
B_SPLINE_CURVE_WITH_KNOTS((3,3),(0.0467199500564191,0.0898699663113548),
 .UNSPECIFIED.)
CURVE()
GEOMETRIC_REPRESENTATION_ITEM()
RATIONAL_B_SPLINE_CURVE((1.00126937543092,1.00122087809464,1.))
REPRESENTATION_ITEM('')
);
#193=(
BOUNDED_CURVE()
B_SPLINE_CURVE(2,(#31165,#31166,#31167),.UNSPECIFIED.,.F.,.F.)
B_SPLINE_CURVE_WITH_KNOTS((3,3),(0.,0.0436887632257914),.UNSPECIFIED.)
CURVE()
GEOMETRIC_REPRESENTATION_ITEM()
RATIONAL_B_SPLINE_CURVE((1.,1.00100330533698,1.0008342561211))
REPRESENTATION_ITEM('')
);
#194=(
BOUNDED_CURVE()
B_SPLINE_CURVE(2,(#31171,#31172,#31173),.UNSPECIFIED.,.F.,.F.)
B_SPLINE_CURVE_WITH_KNOTS((3,3),(0.,0.0431500162549322),.UNSPECIFIED.)
CURVE()
GEOMETRIC_REPRESENTATION_ITEM()
RATIONAL_B_SPLINE_CURVE((1.,1.00122087809449,1.00126937543076))
REPRESENTATION_ITEM('')
);
#195=(
BOUNDED_CURVE()
B_SPLINE_CURVE(2,(#31176,#31177,#31178),.UNSPECIFIED.,.F.,.F.)
B_SPLINE_CURVE_WITH_KNOTS((3,3),(0.0310892451911953,0.0747780084169828),
 .UNSPECIFIED.)
CURVE()
GEOMETRIC_REPRESENTATION_ITEM()
RATIONAL_B_SPLINE_CURVE((1.0008342561224,1.00100330533854,1.))
REPRESENTATION_ITEM('')
);
#196=(
BOUNDED_CURVE()
B_SPLINE_CURVE(2,(#31182,#31183,#31184),.UNSPECIFIED.,.F.,.F.)
B_SPLINE_CURVE_WITH_KNOTS((3,3),(0.0467199500564009,0.0898699663113548),
 .UNSPECIFIED.)
CURVE()
GEOMETRIC_REPRESENTATION_ITEM()
RATIONAL_B_SPLINE_CURVE((1.00126937543082,1.00122087809454,1.))
REPRESENTATION_ITEM('')
);
#197=(
BOUNDED_CURVE()
B_SPLINE_CURVE(2,(#31188,#31189,#31190),.UNSPECIFIED.,.F.,.F.)
B_SPLINE_CURVE_WITH_KNOTS((3,3),(0.,0.04368876322581),.UNSPECIFIED.)
CURVE()
GEOMETRIC_REPRESENTATION_ITEM()
RATIONAL_B_SPLINE_CURVE((1.,1.00100330533771,1.00083425612171))
REPRESENTATION_ITEM('')
);
#198=(
BOUNDED_CURVE()
B_SPLINE_CURVE(2,(#31194,#31195,#31196),.UNSPECIFIED.,.F.,.F.)
B_SPLINE_CURVE_WITH_KNOTS((3,3),(0.,0.0431500162549717),.UNSPECIFIED.)
CURVE()
GEOMETRIC_REPRESENTATION_ITEM()
RATIONAL_B_SPLINE_CURVE((1.,1.00122087809461,1.00126937543088))
REPRESENTATION_ITEM('')
);
#199=(
BOUNDED_CURVE()
B_SPLINE_CURVE(2,(#31199,#31200,#31201),.UNSPECIFIED.,.F.,.F.)
B_SPLINE_CURVE_WITH_KNOTS((3,3),(0.0310892451911806,0.0747780084169829),
 .UNSPECIFIED.)
CURVE()
GEOMETRIC_REPRESENTATION_ITEM()
RATIONAL_B_SPLINE_CURVE((1.00083425612159,1.00100330533756,1.))
REPRESENTATION_ITEM('')
);
#200=(
BOUNDED_CURVE()
B_SPLINE_CURVE(2,(#31205,#31206,#31207),.UNSPECIFIED.,.F.,.F.)
B_SPLINE_CURVE_WITH_KNOTS((3,3),(0.0467199500564204,0.0898699663113548),
 .UNSPECIFIED.)
CURVE()
GEOMETRIC_REPRESENTATION_ITEM()
RATIONAL_B_SPLINE_CURVE((1.00126937543083,1.00122087809455,1.))
REPRESENTATION_ITEM('')
);
#201=(
BOUNDED_CURVE()
B_SPLINE_CURVE(2,(#31211,#31212,#31213),.UNSPECIFIED.,.F.,.F.)
B_SPLINE_CURVE_WITH_KNOTS((3,3),(0.,0.0436887632258064),.UNSPECIFIED.)
CURVE()
GEOMETRIC_REPRESENTATION_ITEM()
RATIONAL_B_SPLINE_CURVE((1.,1.00100330533703,1.00083425612115))
REPRESENTATION_ITEM('')
);
#202=(
BOUNDED_CURVE()
B_SPLINE_CURVE(2,(#31217,#31218,#31219),.UNSPECIFIED.,.F.,.F.)
B_SPLINE_CURVE_WITH_KNOTS((3,3),(0.,0.0431500162549232),.UNSPECIFIED.)
CURVE()
GEOMETRIC_REPRESENTATION_ITEM()
RATIONAL_B_SPLINE_CURVE((1.,1.00122087809502,1.00126937543132))
REPRESENTATION_ITEM('')
);
#203=(
BOUNDED_CURVE()
B_SPLINE_CURVE(2,(#31222,#31223,#31224),.UNSPECIFIED.,.F.,.F.)
B_SPLINE_CURVE_WITH_KNOTS((3,3),(0.0310892451911708,0.0747780084169828),
 .UNSPECIFIED.)
CURVE()
GEOMETRIC_REPRESENTATION_ITEM()
RATIONAL_B_SPLINE_CURVE((1.00083425612115,1.00100330533704,1.))
REPRESENTATION_ITEM('')
);
#204=(
BOUNDED_CURVE()
B_SPLINE_CURVE(2,(#31228,#31229,#31230),.UNSPECIFIED.,.F.,.F.)
B_SPLINE_CURVE_WITH_KNOTS((3,3),(0.04671995005641,0.0898699663113547),
 .UNSPECIFIED.)
CURVE()
GEOMETRIC_REPRESENTATION_ITEM()
RATIONAL_B_SPLINE_CURVE((1.00126937543045,1.00122087809419,1.))
REPRESENTATION_ITEM('')
);
#205=(
BOUNDED_CURVE()
B_SPLINE_CURVE(2,(#31234,#31235,#31236),.UNSPECIFIED.,.F.,.F.)
B_SPLINE_CURVE_WITH_KNOTS((3,3),(0.,0.0436887632258215),.UNSPECIFIED.)
CURVE()
GEOMETRIC_REPRESENTATION_ITEM()
RATIONAL_B_SPLINE_CURVE((1.,1.00100330533736,1.00083425612143))
REPRESENTATION_ITEM('')
);
#206=(
BOUNDED_CURVE()
B_SPLINE_CURVE(2,(#31240,#31241,#31242),.UNSPECIFIED.,.F.,.F.)
B_SPLINE_CURVE_WITH_KNOTS((3,3),(0.,0.0431500162549405),.UNSPECIFIED.)
CURVE()
GEOMETRIC_REPRESENTATION_ITEM()
RATIONAL_B_SPLINE_CURVE((1.,1.00122087809483,1.00126937543112))
REPRESENTATION_ITEM('')
);
#207=(
BOUNDED_CURVE()
B_SPLINE_CURVE(2,(#31245,#31246,#31247),.UNSPECIFIED.,.F.,.F.)
B_SPLINE_CURVE_WITH_KNOTS((3,3),(0.0310892451911933,0.0747780084169829),
 .UNSPECIFIED.)
CURVE()
GEOMETRIC_REPRESENTATION_ITEM()
RATIONAL_B_SPLINE_CURVE((1.00083425612156,1.00100330533752,1.))
REPRESENTATION_ITEM('')
);
#208=(
BOUNDED_CURVE()
B_SPLINE_CURVE(2,(#31251,#31252,#31253),.UNSPECIFIED.,.F.,.F.)
B_SPLINE_CURVE_WITH_KNOTS((3,3),(0.0467199500564031,0.0898699663113549),
 .UNSPECIFIED.)
CURVE()
GEOMETRIC_REPRESENTATION_ITEM()
RATIONAL_B_SPLINE_CURVE((1.00126937543121,1.00122087809492,1.))
REPRESENTATION_ITEM('')
);
#209=(
BOUNDED_CURVE()
B_SPLINE_CURVE(2,(#31257,#31258,#31259),.UNSPECIFIED.,.F.,.F.)
B_SPLINE_CURVE_WITH_KNOTS((3,3),(0.,0.0436887632258158),.UNSPECIFIED.)
CURVE()
GEOMETRIC_REPRESENTATION_ITEM()
RATIONAL_B_SPLINE_CURVE((1.,1.0010033053384,1.00083425612229))
REPRESENTATION_ITEM('')
);
#210=(
BOUNDED_CURVE()
B_SPLINE_CURVE(2,(#31263,#31264,#31265),.UNSPECIFIED.,.F.,.F.)
B_SPLINE_CURVE_WITH_KNOTS((3,3),(0.,0.0431500162549452),.UNSPECIFIED.)
CURVE()
GEOMETRIC_REPRESENTATION_ITEM()
RATIONAL_B_SPLINE_CURVE((1.,1.00122087809455,1.00126937543082))
REPRESENTATION_ITEM('')
);
#211=(
BOUNDED_CURVE()
B_SPLINE_CURVE(2,(#31268,#31269,#31270),.UNSPECIFIED.,.F.,.F.)
B_SPLINE_CURVE_WITH_KNOTS((3,3),(0.0310892451911938,0.0747780084169828),
 .UNSPECIFIED.)
CURVE()
GEOMETRIC_REPRESENTATION_ITEM()
RATIONAL_B_SPLINE_CURVE((1.00083425612169,1.00100330533769,1.))
REPRESENTATION_ITEM('')
);
#212=(
BOUNDED_CURVE()
B_SPLINE_CURVE(2,(#31274,#31275,#31276),.UNSPECIFIED.,.F.,.F.)
B_SPLINE_CURVE_WITH_KNOTS((3,3),(0.0467199500564215,0.0898699663113548),
 .UNSPECIFIED.)
CURVE()
GEOMETRIC_REPRESENTATION_ITEM()
RATIONAL_B_SPLINE_CURVE((1.00126937543076,1.00122087809448,1.))
REPRESENTATION_ITEM('')
);
#213=(
BOUNDED_CURVE()
B_SPLINE_CURVE(2,(#31280,#31281,#31282),.UNSPECIFIED.,.F.,.F.)
B_SPLINE_CURVE_WITH_KNOTS((3,3),(0.,0.0436887632258074),.UNSPECIFIED.)
CURVE()
GEOMETRIC_REPRESENTATION_ITEM()
RATIONAL_B_SPLINE_CURVE((1.,1.00100330533774,1.00083425612174))
REPRESENTATION_ITEM('')
);
#214=(
BOUNDED_CURVE()
B_SPLINE_CURVE(2,(#31286,#31287,#31288),.UNSPECIFIED.,.F.,.F.)
B_SPLINE_CURVE_WITH_KNOTS((3,3),(0.,0.0431500162549509),.UNSPECIFIED.)
CURVE()
GEOMETRIC_REPRESENTATION_ITEM()
RATIONAL_B_SPLINE_CURVE((1.,1.00122087809425,1.00126937543051))
REPRESENTATION_ITEM('')
);
#215=(
BOUNDED_CURVE()
B_SPLINE_CURVE(2,(#31291,#31292,#31293),.UNSPECIFIED.,.F.,.F.)
B_SPLINE_CURVE_WITH_KNOTS((3,3),(0.0310892451912129,0.0747780084169828),
 .UNSPECIFIED.)
CURVE()
GEOMETRIC_REPRESENTATION_ITEM()
RATIONAL_B_SPLINE_CURVE((1.00083425612163,1.00100330533761,1.))
REPRESENTATION_ITEM('')
);
#216=(
BOUNDED_CURVE()
B_SPLINE_CURVE(2,(#31297,#31298,#31299),.UNSPECIFIED.,.F.,.F.)
B_SPLINE_CURVE_WITH_KNOTS((3,3),(0.0467199500564181,0.0898699663113547),
 .UNSPECIFIED.)
CURVE()
GEOMETRIC_REPRESENTATION_ITEM()
RATIONAL_B_SPLINE_CURVE((1.00126937543066,1.0012208780944,1.))
REPRESENTATION_ITEM('')
);
#217=(
BOUNDED_CURVE()
B_SPLINE_CURVE(2,(#31303,#31304,#31305),.UNSPECIFIED.,.F.,.F.)
B_SPLINE_CURVE_WITH_KNOTS((3,3),(0.,0.0436887632258064),.UNSPECIFIED.)
CURVE()
GEOMETRIC_REPRESENTATION_ITEM()
RATIONAL_B_SPLINE_CURVE((1.,1.00100330533711,1.00083425612121))
REPRESENTATION_ITEM('')
);
#218=(
BOUNDED_CURVE()
B_SPLINE_CURVE(2,(#31309,#31310,#31311),.UNSPECIFIED.,.F.,.F.)
B_SPLINE_CURVE_WITH_KNOTS((3,3),(0.,0.0431500162549468),.UNSPECIFIED.)
CURVE()
GEOMETRIC_REPRESENTATION_ITEM()
RATIONAL_B_SPLINE_CURVE((1.,1.00122087809451,1.00126937543078))
REPRESENTATION_ITEM('')
);
#219=(
BOUNDED_CURVE()
B_SPLINE_CURVE(2,(#31314,#31315,#31316),.UNSPECIFIED.,.F.,.F.)
B_SPLINE_CURVE_WITH_KNOTS((3,3),(0.0310892451911651,0.0747780084169829),
 .UNSPECIFIED.)
CURVE()
GEOMETRIC_REPRESENTATION_ITEM()
RATIONAL_B_SPLINE_CURVE((1.00083425612205,1.00100330533812,1.))
REPRESENTATION_ITEM('')
);
#220=(
BOUNDED_CURVE()
B_SPLINE_CURVE(2,(#31320,#31321,#31322),.UNSPECIFIED.,.F.,.F.)
B_SPLINE_CURVE_WITH_KNOTS((3,3),(0.0467199500563987,0.0898699663113548),
 .UNSPECIFIED.)
CURVE()
GEOMETRIC_REPRESENTATION_ITEM()
RATIONAL_B_SPLINE_CURVE((1.00126937543082,1.00122087809454,1.))
REPRESENTATION_ITEM('')
);
#221=(
BOUNDED_CURVE()
B_SPLINE_CURVE(2,(#31326,#31327,#31328),.UNSPECIFIED.,.F.,.F.)
B_SPLINE_CURVE_WITH_KNOTS((3,3),(0.,0.0436887632257942),.UNSPECIFIED.)
CURVE()
GEOMETRIC_REPRESENTATION_ITEM()
RATIONAL_B_SPLINE_CURVE((1.,1.0010033053377,1.0008342561217))
REPRESENTATION_ITEM('')
);
#222=(
BOUNDED_CURVE()
B_SPLINE_CURVE(2,(#31332,#31333,#31334),.UNSPECIFIED.,.F.,.F.)
B_SPLINE_CURVE_WITH_KNOTS((3,3),(0.,0.0431500162549576),.UNSPECIFIED.)
CURVE()
GEOMETRIC_REPRESENTATION_ITEM()
RATIONAL_B_SPLINE_CURVE((1.,1.00122087809465,1.00126937543093))
REPRESENTATION_ITEM('')
);
#223=(
BOUNDED_CURVE()
B_SPLINE_CURVE(2,(#31337,#31338,#31339),.UNSPECIFIED.,.F.,.F.)
B_SPLINE_CURVE_WITH_KNOTS((3,3),(0.0310892451911712,0.0747780084169828),
 .UNSPECIFIED.)
CURVE()
GEOMETRIC_REPRESENTATION_ITEM()
RATIONAL_B_SPLINE_CURVE((1.00083425612158,1.00100330533755,1.))
REPRESENTATION_ITEM('')
);
#224=(
BOUNDED_CURVE()
B_SPLINE_CURVE(2,(#31343,#31344,#31345),.UNSPECIFIED.,.F.,.F.)
B_SPLINE_CURVE_WITH_KNOTS((3,3),(0.0467199500563997,0.0898699663113548),
 .UNSPECIFIED.)
CURVE()
GEOMETRIC_REPRESENTATION_ITEM()
RATIONAL_B_SPLINE_CURVE((1.00126937543088,1.0012208780946,1.))
REPRESENTATION_ITEM('')
);
#225=(
BOUNDED_CURVE()
B_SPLINE_CURVE(2,(#31349,#31350,#31351),.UNSPECIFIED.,.F.,.F.)
B_SPLINE_CURVE_WITH_KNOTS((3,3),(0.,0.0436887632257912),.UNSPECIFIED.)
CURVE()
GEOMETRIC_REPRESENTATION_ITEM()
RATIONAL_B_SPLINE_CURVE((1.,1.00100330533807,1.00083425612201))
REPRESENTATION_ITEM('')
);
#226=(
BOUNDED_CURVE()
B_SPLINE_CURVE(2,(#31355,#31356,#31357),.UNSPECIFIED.,.F.,.F.)
B_SPLINE_CURVE_WITH_KNOTS((3,3),(0.,0.0431500162549322),.UNSPECIFIED.)
CURVE()
GEOMETRIC_REPRESENTATION_ITEM()
RATIONAL_B_SPLINE_CURVE((1.,1.00122087809449,1.00126937543076))
REPRESENTATION_ITEM('')
);
#227=(
BOUNDED_CURVE()
B_SPLINE_CURVE(2,(#31360,#31361,#31362),.UNSPECIFIED.,.F.,.F.)
B_SPLINE_CURVE_WITH_KNOTS((3,3),(0.0310892451911953,0.0747780084169828),
 .UNSPECIFIED.)
CURVE()
GEOMETRIC_REPRESENTATION_ITEM()
RATIONAL_B_SPLINE_CURVE((1.0008342561224,1.00100330533854,1.))
REPRESENTATION_ITEM('')
);
#228=(
BOUNDED_CURVE()
B_SPLINE_CURVE(2,(#31366,#31367,#31368),.UNSPECIFIED.,.F.,.F.)
B_SPLINE_CURVE_WITH_KNOTS((3,3),(0.0467199500563888,0.0898699663113548),
 .UNSPECIFIED.)
CURVE()
GEOMETRIC_REPRESENTATION_ITEM()
RATIONAL_B_SPLINE_CURVE((1.0012693754306,1.00122087809433,1.))
REPRESENTATION_ITEM('')
);
#229=(
BOUNDED_CURVE()
B_SPLINE_CURVE(2,(#31372,#31373,#31374),.UNSPECIFIED.,.F.,.F.)
B_SPLINE_CURVE_WITH_KNOTS((3,3),(0.,0.0436887632258443),.UNSPECIFIED.)
CURVE()
GEOMETRIC_REPRESENTATION_ITEM()
RATIONAL_B_SPLINE_CURVE((1.,1.00100330533721,1.0008342561213))
REPRESENTATION_ITEM('')
);
#230=(
BOUNDED_CURVE()
B_SPLINE_CURVE(2,(#31378,#31379,#31380),.UNSPECIFIED.,.F.,.F.)
B_SPLINE_CURVE_WITH_KNOTS((3,3),(0.,0.0431500162549717),.UNSPECIFIED.)
CURVE()
GEOMETRIC_REPRESENTATION_ITEM()
RATIONAL_B_SPLINE_CURVE((1.,1.00122087809461,1.00126937543088))
REPRESENTATION_ITEM('')
);
#231=(
BOUNDED_CURVE()
B_SPLINE_CURVE(2,(#31383,#31384,#31385),.UNSPECIFIED.,.F.,.F.)
B_SPLINE_CURVE_WITH_KNOTS((3,3),(0.0310892451911806,0.0747780084169829),
 .UNSPECIFIED.)
CURVE()
GEOMETRIC_REPRESENTATION_ITEM()
RATIONAL_B_SPLINE_CURVE((1.00083425612159,1.00100330533756,1.))
REPRESENTATION_ITEM('')
);
#232=(
BOUNDED_CURVE()
B_SPLINE_CURVE(2,(#31389,#31390,#31391),.UNSPECIFIED.,.F.,.F.)
B_SPLINE_CURVE_WITH_KNOTS((3,3),(0.0467199500563954,0.0898699663113548),
 .UNSPECIFIED.)
CURVE()
GEOMETRIC_REPRESENTATION_ITEM()
RATIONAL_B_SPLINE_CURVE((1.00126937543089,1.00122087809461,1.))
REPRESENTATION_ITEM('')
);
#233=(
BOUNDED_CURVE()
B_SPLINE_CURVE(2,(#31395,#31396,#31397),.UNSPECIFIED.,.F.,.F.)
B_SPLINE_CURVE_WITH_KNOTS((3,3),(0.,0.0436887632258089),.UNSPECIFIED.)
CURVE()
GEOMETRIC_REPRESENTATION_ITEM()
RATIONAL_B_SPLINE_CURVE((1.,1.00100330533773,1.00083425612173))
REPRESENTATION_ITEM('')
);
#234=(
BOUNDED_CURVE()
B_SPLINE_CURVE(2,(#31401,#31402,#31403),.UNSPECIFIED.,.F.,.F.)
B_SPLINE_CURVE_WITH_KNOTS((3,3),(0.,0.0431500162549499),.UNSPECIFIED.)
CURVE()
GEOMETRIC_REPRESENTATION_ITEM()
RATIONAL_B_SPLINE_CURVE((1.,1.00122087809471,1.00126937543099))
REPRESENTATION_ITEM('')
);
#235=(
BOUNDED_CURVE()
B_SPLINE_CURVE(2,(#31406,#31407,#31408),.UNSPECIFIED.,.F.,.F.)
B_SPLINE_CURVE_WITH_KNOTS((3,3),(0.0310892451911691,0.0747780084169828),
 .UNSPECIFIED.)
CURVE()
GEOMETRIC_REPRESENTATION_ITEM()
RATIONAL_B_SPLINE_CURVE((1.0008342561213,1.00100330533722,1.))
REPRESENTATION_ITEM('')
);
#236=(
BOUNDED_CURVE()
B_SPLINE_CURVE(2,(#31412,#31413,#31414),.UNSPECIFIED.,.F.,.F.)
B_SPLINE_CURVE_WITH_KNOTS((3,3),(0.0467199500563946,0.0898699663113549),
 .UNSPECIFIED.)
CURVE()
GEOMETRIC_REPRESENTATION_ITEM()
RATIONAL_B_SPLINE_CURVE((1.00126937543091,1.00122087809463,1.))
REPRESENTATION_ITEM('')
);
#237=(
BOUNDED_CURVE()
B_SPLINE_CURVE(2,(#31418,#31419,#31420),.UNSPECIFIED.,.F.,.F.)
B_SPLINE_CURVE_WITH_KNOTS((3,3),(0.,0.0436887632258018),.UNSPECIFIED.)
CURVE()
GEOMETRIC_REPRESENTATION_ITEM()
RATIONAL_B_SPLINE_CURVE((1.,1.00100330533801,1.00083425612196))
REPRESENTATION_ITEM('')
);
#238=(
BOUNDED_CURVE()
B_SPLINE_CURVE(2,(#31424,#31425,#31426),.UNSPECIFIED.,.F.,.F.)
B_SPLINE_CURVE_WITH_KNOTS((3,3),(0.,0.0431500162549446),.UNSPECIFIED.)
CURVE()
GEOMETRIC_REPRESENTATION_ITEM()
RATIONAL_B_SPLINE_CURVE((1.,1.00122087809491,1.00126937543119))
REPRESENTATION_ITEM('')
);
#239=(
BOUNDED_CURVE()
B_SPLINE_CURVE(2,(#31429,#31430,#31431),.UNSPECIFIED.,.F.,.F.)
B_SPLINE_CURVE_WITH_KNOTS((3,3),(0.0310892451912006,0.0747780084169829),
 .UNSPECIFIED.)
CURVE()
GEOMETRIC_REPRESENTATION_ITEM()
RATIONAL_B_SPLINE_CURVE((1.00083425612167,1.00100330533765,1.))
REPRESENTATION_ITEM('')
);
#240=(
BOUNDED_CURVE()
B_SPLINE_CURVE(2,(#31435,#31436,#31437),.UNSPECIFIED.,.F.,.F.)
B_SPLINE_CURVE_WITH_KNOTS((3,3),(0.0467199500564005,0.0898699663113549),
 .UNSPECIFIED.)
CURVE()
GEOMETRIC_REPRESENTATION_ITEM()
RATIONAL_B_SPLINE_CURVE((1.00126937543091,1.00122087809463,1.))
REPRESENTATION_ITEM('')
);
#241=(
BOUNDED_CURVE()
B_SPLINE_CURVE(2,(#31441,#31442,#31443),.UNSPECIFIED.,.F.,.F.)
B_SPLINE_CURVE_WITH_KNOTS((3,3),(0.,0.0436887632257904),.UNSPECIFIED.)
CURVE()
GEOMETRIC_REPRESENTATION_ITEM()
RATIONAL_B_SPLINE_CURVE((1.,1.00100330533768,1.00083425612169))
REPRESENTATION_ITEM('')
);
#242=(
BOUNDED_CURVE()
B_SPLINE_CURVE(2,(#31447,#31448,#31449),.UNSPECIFIED.,.F.,.F.)
B_SPLINE_CURVE_WITH_KNOTS((3,3),(0.,0.0431500162549576),.UNSPECIFIED.)
CURVE()
GEOMETRIC_REPRESENTATION_ITEM()
RATIONAL_B_SPLINE_CURVE((1.,1.00122087809446,1.00126937543073))
REPRESENTATION_ITEM('')
);
#243=(
BOUNDED_CURVE()
B_SPLINE_CURVE(2,(#31452,#31453,#31454),.UNSPECIFIED.,.F.,.F.)
B_SPLINE_CURVE_WITH_KNOTS((3,3),(0.0310892451911633,0.0747780084169828),
 .UNSPECIFIED.)
CURVE()
GEOMETRIC_REPRESENTATION_ITEM()
RATIONAL_B_SPLINE_CURVE((1.00083425612268,1.00100330533887,1.))
REPRESENTATION_ITEM('')
);
#244=(
BOUNDED_CURVE()
B_SPLINE_CURVE(2,(#31458,#31459,#31460),.UNSPECIFIED.,.F.,.F.)
B_SPLINE_CURVE_WITH_KNOTS((3,3),(0.0467199500564166,0.089869966311355),
 .UNSPECIFIED.)
CURVE()
GEOMETRIC_REPRESENTATION_ITEM()
RATIONAL_B_SPLINE_CURVE((1.00126937543126,1.00122087809497,1.))
REPRESENTATION_ITEM('')
);
#245=(
BOUNDED_CURVE()
B_SPLINE_CURVE(2,(#31464,#31465,#31466),.UNSPECIFIED.,.F.,.F.)
B_SPLINE_CURVE_WITH_KNOTS((3,3),(0.,0.0436887632258151),.UNSPECIFIED.)
CURVE()
GEOMETRIC_REPRESENTATION_ITEM()
RATIONAL_B_SPLINE_CURVE((1.,1.00100330533817,1.00083425612209))
REPRESENTATION_ITEM('')
);
#246=(
BOUNDED_CURVE()
B_SPLINE_CURVE(2,(#31470,#31471,#31472),.UNSPECIFIED.,.F.,.F.)
B_SPLINE_CURVE_WITH_KNOTS((3,3),(0.,0.0431500162549457),.UNSPECIFIED.)
CURVE()
GEOMETRIC_REPRESENTATION_ITEM()
RATIONAL_B_SPLINE_CURVE((1.,1.00122087809449,1.00126937543076))
REPRESENTATION_ITEM('')
);
#247=(
BOUNDED_CURVE()
B_SPLINE_CURVE(2,(#31475,#31476,#31477),.UNSPECIFIED.,.F.,.F.)
B_SPLINE_CURVE_WITH_KNOTS((3,3),(0.0310892451911691,0.0747780084169829),
 .UNSPECIFIED.)
CURVE()
GEOMETRIC_REPRESENTATION_ITEM()
RATIONAL_B_SPLINE_CURVE((1.00083425612148,1.00100330533743,1.))
REPRESENTATION_ITEM('')
);
#248=(
BOUNDED_CURVE()
B_SPLINE_CURVE(2,(#31481,#31482,#31483),.UNSPECIFIED.,.F.,.F.)
B_SPLINE_CURVE_WITH_KNOTS((3,3),(0.0467199500564313,0.089869966311355),
 .UNSPECIFIED.)
CURVE()
GEOMETRIC_REPRESENTATION_ITEM()
RATIONAL_B_SPLINE_CURVE((1.00126937543075,1.00122087809448,1.))
REPRESENTATION_ITEM('')
);
#249=(
BOUNDED_CURVE()
B_SPLINE_CURVE(2,(#31487,#31488,#31489),.UNSPECIFIED.,.F.,.F.)
B_SPLINE_CURVE_WITH_KNOTS((3,3),(0.,0.0436887632257837),.UNSPECIFIED.)
CURVE()
GEOMETRIC_REPRESENTATION_ITEM()
RATIONAL_B_SPLINE_CURVE((1.,1.00100330533754,1.00083425612157))
REPRESENTATION_ITEM('')
);
#250=(
BOUNDED_CURVE()
B_SPLINE_CURVE(2,(#31493,#31494,#31495),.UNSPECIFIED.,.F.,.F.)
B_SPLINE_CURVE_WITH_KNOTS((3,3),(0.,0.043150016254948),.UNSPECIFIED.)
CURVE()
GEOMETRIC_REPRESENTATION_ITEM()
RATIONAL_B_SPLINE_CURVE((1.,1.00122087809439,1.00126937543066))
REPRESENTATION_ITEM('')
);
#251=(
BOUNDED_CURVE()
B_SPLINE_CURVE(2,(#31498,#31499,#31500),.UNSPECIFIED.,.F.,.F.)
B_SPLINE_CURVE_WITH_KNOTS((3,3),(0.0310892451912077,0.0747780084169828),
 .UNSPECIFIED.)
CURVE()
GEOMETRIC_REPRESENTATION_ITEM()
RATIONAL_B_SPLINE_CURVE((1.00083425612152,1.00100330533748,1.))
REPRESENTATION_ITEM('')
);
#252=(
BOUNDED_CURVE()
B_SPLINE_CURVE(2,(#35550,#35551,#35552),.UNSPECIFIED.,.F.,.F.)
B_SPLINE_CURVE_WITH_KNOTS((3,3),(0.,0.00349669843186121),.UNSPECIFIED.)
CURVE()
GEOMETRIC_REPRESENTATION_ITEM()
RATIONAL_B_SPLINE_CURVE((1.,1.00004723091695,1.))
REPRESENTATION_ITEM('')
);
#253=(
BOUNDED_CURVE()
B_SPLINE_CURVE(2,(#35554,#35555,#35556),.UNSPECIFIED.,.F.,.F.)
B_SPLINE_CURVE_WITH_KNOTS((3,3),(0.,0.00349669843186122),.UNSPECIFIED.)
CURVE()
GEOMETRIC_REPRESENTATION_ITEM()
RATIONAL_B_SPLINE_CURVE((1.,1.00004723094136,1.))
REPRESENTATION_ITEM('')
);
#254=(
BOUNDED_CURVE()
B_SPLINE_CURVE(2,(#35559,#35560,#35561),.UNSPECIFIED.,.F.,.F.)
B_SPLINE_CURVE_WITH_KNOTS((3,3),(0.,0.00349669843186136),.UNSPECIFIED.)
CURVE()
GEOMETRIC_REPRESENTATION_ITEM()
RATIONAL_B_SPLINE_CURVE((1.,1.00004723092143,1.))
REPRESENTATION_ITEM('')
);
#255=(
BOUNDED_CURVE()
B_SPLINE_CURVE(2,(#35563,#35564,#35565),.UNSPECIFIED.,.F.,.F.)
B_SPLINE_CURVE_WITH_KNOTS((3,3),(0.,0.00349669843186135),.UNSPECIFIED.)
CURVE()
GEOMETRIC_REPRESENTATION_ITEM()
RATIONAL_B_SPLINE_CURVE((1.,1.00004723092493,1.))
REPRESENTATION_ITEM('')
);
#256=(
BOUNDED_CURVE()
B_SPLINE_CURVE(2,(#35568,#35569,#35570),.UNSPECIFIED.,.F.,.F.)
B_SPLINE_CURVE_WITH_KNOTS((3,3),(0.,0.00349669843186138),.UNSPECIFIED.)
CURVE()
GEOMETRIC_REPRESENTATION_ITEM()
RATIONAL_B_SPLINE_CURVE((1.,1.00004723092744,1.))
REPRESENTATION_ITEM('')
);
#257=(
BOUNDED_CURVE()
B_SPLINE_CURVE(2,(#35572,#35573,#35574),.UNSPECIFIED.,.F.,.F.)
B_SPLINE_CURVE_WITH_KNOTS((3,3),(0.,0.00349669843186141),.UNSPECIFIED.)
CURVE()
GEOMETRIC_REPRESENTATION_ITEM()
RATIONAL_B_SPLINE_CURVE((1.,1.00004723090855,1.))
REPRESENTATION_ITEM('')
);
#258=(
BOUNDED_CURVE()
B_SPLINE_CURVE(2,(#35577,#35578,#35579),.UNSPECIFIED.,.F.,.F.)
B_SPLINE_CURVE_WITH_KNOTS((3,3),(0.,0.0034966984318615),.UNSPECIFIED.)
CURVE()
GEOMETRIC_REPRESENTATION_ITEM()
RATIONAL_B_SPLINE_CURVE((1.,1.00004723094741,1.))
REPRESENTATION_ITEM('')
);
#259=(
BOUNDED_CURVE()
B_SPLINE_CURVE(2,(#35581,#35582,#35583),.UNSPECIFIED.,.F.,.F.)
B_SPLINE_CURVE_WITH_KNOTS((3,3),(0.,0.00349669843186142),.UNSPECIFIED.)
CURVE()
GEOMETRIC_REPRESENTATION_ITEM()
RATIONAL_B_SPLINE_CURVE((1.,1.00004723090666,1.))
REPRESENTATION_ITEM('')
);
#260=(
BOUNDED_CURVE()
B_SPLINE_CURVE(2,(#35586,#35587,#35588),.UNSPECIFIED.,.F.,.F.)
B_SPLINE_CURVE_WITH_KNOTS((3,3),(0.,0.00349669843186135),.UNSPECIFIED.)
CURVE()
GEOMETRIC_REPRESENTATION_ITEM()
RATIONAL_B_SPLINE_CURVE((1.,1.0000472309119,1.))
REPRESENTATION_ITEM('')
);
#261=(
BOUNDED_CURVE()
B_SPLINE_CURVE(2,(#35590,#35591,#35592),.UNSPECIFIED.,.F.,.F.)
B_SPLINE_CURVE_WITH_KNOTS((3,3),(0.,0.00349669843186137),.UNSPECIFIED.)
CURVE()
GEOMETRIC_REPRESENTATION_ITEM()
RATIONAL_B_SPLINE_CURVE((1.,1.00004723093721,1.))
REPRESENTATION_ITEM('')
);
#262=(
BOUNDED_CURVE()
B_SPLINE_CURVE(2,(#35595,#35596,#35597),.UNSPECIFIED.,.F.,.F.)
B_SPLINE_CURVE_WITH_KNOTS((3,3),(0.,0.00349669843186128),.UNSPECIFIED.)
CURVE()
GEOMETRIC_REPRESENTATION_ITEM()
RATIONAL_B_SPLINE_CURVE((1.,1.00004723093599,1.))
REPRESENTATION_ITEM('')
);
#263=(
BOUNDED_CURVE()
B_SPLINE_CURVE(2,(#35599,#35600,#35601),.UNSPECIFIED.,.F.,.F.)
B_SPLINE_CURVE_WITH_KNOTS((3,3),(0.,0.00349669843186128),.UNSPECIFIED.)
CURVE()
GEOMETRIC_REPRESENTATION_ITEM()
RATIONAL_B_SPLINE_CURVE((1.,1.00004723092625,1.))
REPRESENTATION_ITEM('')
);
#264=(
BOUNDED_CURVE()
B_SPLINE_CURVE(2,(#35672,#35673,#35674),.UNSPECIFIED.,.F.,.F.)
B_SPLINE_CURVE_WITH_KNOTS((3,3),(0.0420809670913651,0.0588848364681992),
 .UNSPECIFIED.)
CURVE()
GEOMETRIC_REPRESENTATION_ITEM()
RATIONAL_B_SPLINE_CURVE((1.00087707567824,1.00061365578614,1.))
REPRESENTATION_ITEM('')
);
#265=(
BOUNDED_CURVE()
B_SPLINE_CURVE(2,(#35679,#35680,#35681),.UNSPECIFIED.,.F.,.F.)
B_SPLINE_CURVE_WITH_KNOTS((3,3),(0.,0.0168038693768593),.UNSPECIFIED.)
CURVE()
GEOMETRIC_REPRESENTATION_ITEM()
RATIONAL_B_SPLINE_CURVE((1.,1.00061365578593,1.00087707567795))
REPRESENTATION_ITEM('')
);
#266=(
BOUNDED_CURVE()
B_SPLINE_CURVE(2,(#35686,#35687,#35688),.UNSPECIFIED.,.F.,.F.)
B_SPLINE_CURVE_WITH_KNOTS((3,3),(0.0420809670913399,0.0588848364681993),
 .UNSPECIFIED.)
CURVE()
GEOMETRIC_REPRESENTATION_ITEM()
RATIONAL_B_SPLINE_CURVE((1.00087707567746,1.00061365578559,1.))
REPRESENTATION_ITEM('')
);
#267=(
BOUNDED_CURVE()
B_SPLINE_CURVE(2,(#35693,#35694,#35695),.UNSPECIFIED.,.F.,.F.)
B_SPLINE_CURVE_WITH_KNOTS((3,3),(0.,0.0168038693768394),.UNSPECIFIED.)
CURVE()
GEOMETRIC_REPRESENTATION_ITEM()
RATIONAL_B_SPLINE_CURVE((1.,1.00061365578594,1.00087707567797))
REPRESENTATION_ITEM('')
);
#268=(
BOUNDED_CURVE()
B_SPLINE_CURVE(2,(#35700,#35701,#35702),.UNSPECIFIED.,.F.,.F.)
B_SPLINE_CURVE_WITH_KNOTS((3,3),(0.0420809670913626,0.0588848364681992),
 .UNSPECIFIED.)
CURVE()
GEOMETRIC_REPRESENTATION_ITEM()
RATIONAL_B_SPLINE_CURVE((1.00087707567775,1.00061365578579,1.))
REPRESENTATION_ITEM('')
);
#269=(
BOUNDED_CURVE()
B_SPLINE_CURVE(2,(#35707,#35708,#35709),.UNSPECIFIED.,.F.,.F.)
B_SPLINE_CURVE_WITH_KNOTS((3,3),(0.,0.0168038693768627),.UNSPECIFIED.)
CURVE()
GEOMETRIC_REPRESENTATION_ITEM()
RATIONAL_B_SPLINE_CURVE((1.,1.00061365578587,1.00087707567786))
REPRESENTATION_ITEM('')
);
#270=(
BOUNDED_CURVE()
B_SPLINE_CURVE(2,(#35714,#35715,#35716),.UNSPECIFIED.,.F.,.F.)
B_SPLINE_CURVE_WITH_KNOTS((3,3),(0.042080967091394,0.0588848364681993),
 .UNSPECIFIED.)
CURVE()
GEOMETRIC_REPRESENTATION_ITEM()
RATIONAL_B_SPLINE_CURVE((1.00087707567792,1.00061365578591,1.))
REPRESENTATION_ITEM('')
);
#271=(
BOUNDED_CURVE()
B_SPLINE_CURVE(2,(#35721,#35722,#35723),.UNSPECIFIED.,.F.,.F.)
B_SPLINE_CURVE_WITH_KNOTS((3,3),(0.,0.0168038693768566),.UNSPECIFIED.)
CURVE()
GEOMETRIC_REPRESENTATION_ITEM()
RATIONAL_B_SPLINE_CURVE((1.,1.00061365578555,1.0008770756774))
REPRESENTATION_ITEM('')
);
#272=(
BOUNDED_CURVE()
B_SPLINE_CURVE(2,(#35728,#35729,#35730),.UNSPECIFIED.,.F.,.F.)
B_SPLINE_CURVE_WITH_KNOTS((3,3),(0.0420809670913884,0.0588848364681993),
 .UNSPECIFIED.)
CURVE()
GEOMETRIC_REPRESENTATION_ITEM()
RATIONAL_B_SPLINE_CURVE((1.00087707567863,1.0006136557864,1.))
REPRESENTATION_ITEM('')
);
#273=(
BOUNDED_CURVE()
B_SPLINE_CURVE(2,(#35735,#35736,#35737),.UNSPECIFIED.,.F.,.F.)
B_SPLINE_CURVE_WITH_KNOTS((3,3),(0.,0.0168038693768499),.UNSPECIFIED.)
CURVE()
GEOMETRIC_REPRESENTATION_ITEM()
RATIONAL_B_SPLINE_CURVE((1.,1.00061365578631,1.00087707567849))
REPRESENTATION_ITEM('')
);
#274=(
BOUNDED_CURVE()
B_SPLINE_CURVE(2,(#35742,#35743,#35744),.UNSPECIFIED.,.F.,.F.)
B_SPLINE_CURVE_WITH_KNOTS((3,3),(0.0420809670913347,0.0588848364681992),
 .UNSPECIFIED.)
CURVE()
GEOMETRIC_REPRESENTATION_ITEM()
RATIONAL_B_SPLINE_CURVE((1.00087707567759,1.00061365578568,1.))
REPRESENTATION_ITEM('')
);
#275=(
BOUNDED_CURVE()
B_SPLINE_CURVE(2,(#35749,#35750,#35751),.UNSPECIFIED.,.F.,.F.)
B_SPLINE_CURVE_WITH_KNOTS((3,3),(0.,0.0168038693768258),.UNSPECIFIED.)
CURVE()
GEOMETRIC_REPRESENTATION_ITEM()
RATIONAL_B_SPLINE_CURVE((1.,1.00061365578592,1.00087707567793))
REPRESENTATION_ITEM('')
);
#276=(
BOUNDED_CURVE()
B_SPLINE_CURVE(2,(#35756,#35757,#35758),.UNSPECIFIED.,.F.,.F.)
B_SPLINE_CURVE_WITH_KNOTS((3,3),(0.0420809670913505,0.0588848364681993),
 .UNSPECIFIED.)
CURVE()
GEOMETRIC_REPRESENTATION_ITEM()
RATIONAL_B_SPLINE_CURVE((1.00087707567804,1.00061365578599,1.))
REPRESENTATION_ITEM('')
);
#277=(
BOUNDED_CURVE()
B_SPLINE_CURVE(2,(#35763,#35764,#35765),.UNSPECIFIED.,.F.,.F.)
B_SPLINE_CURVE_WITH_KNOTS((3,3),(0.,0.0168038693768362),.UNSPECIFIED.)
CURVE()
GEOMETRIC_REPRESENTATION_ITEM()
RATIONAL_B_SPLINE_CURVE((1.,1.00061365578568,1.00087707567759))
REPRESENTATION_ITEM('')
);
#278=(
BOUNDED_CURVE()
B_SPLINE_CURVE(2,(#35770,#35771,#35772),.UNSPECIFIED.,.F.,.F.)
B_SPLINE_CURVE_WITH_KNOTS((3,3),(0.0420809670913562,0.0588848364681992),
 .UNSPECIFIED.)
CURVE()
GEOMETRIC_REPRESENTATION_ITEM()
RATIONAL_B_SPLINE_CURVE((1.00087707567804,1.00061365578599,1.))
REPRESENTATION_ITEM('')
);
#279=(
BOUNDED_CURVE()
B_SPLINE_CURVE(2,(#35777,#35778,#35779),.UNSPECIFIED.,.F.,.F.)
B_SPLINE_CURVE_WITH_KNOTS((3,3),(0.,0.016803869376823),.UNSPECIFIED.)
CURVE()
GEOMETRIC_REPRESENTATION_ITEM()
RATIONAL_B_SPLINE_CURVE((1.,1.00061365578592,1.00087707567794))
REPRESENTATION_ITEM('')
);
#280=(
BOUNDED_CURVE()
B_SPLINE_CURVE(2,(#35784,#35785,#35786),.UNSPECIFIED.,.F.,.F.)
B_SPLINE_CURVE_WITH_KNOTS((3,3),(0.04208096709136,0.0588848364681992),
 .UNSPECIFIED.)
CURVE()
GEOMETRIC_REPRESENTATION_ITEM()
RATIONAL_B_SPLINE_CURVE((1.00087707567819,1.0006136557861,1.))
REPRESENTATION_ITEM('')
);
#281=(
BOUNDED_CURVE()
B_SPLINE_CURVE(2,(#35791,#35792,#35793),.UNSPECIFIED.,.F.,.F.)
B_SPLINE_CURVE_WITH_KNOTS((3,3),(0.,0.0168038693767949),.UNSPECIFIED.)
CURVE()
GEOMETRIC_REPRESENTATION_ITEM()
RATIONAL_B_SPLINE_CURVE((1.,1.00061365578653,1.00087707567881))
REPRESENTATION_ITEM('')
);
#282=(
BOUNDED_CURVE()
B_SPLINE_CURVE(2,(#35798,#35799,#35800),.UNSPECIFIED.,.F.,.F.)
B_SPLINE_CURVE_WITH_KNOTS((3,3),(0.0420809670913836,0.0588848364681992),
 .UNSPECIFIED.)
CURVE()
GEOMETRIC_REPRESENTATION_ITEM()
RATIONAL_B_SPLINE_CURVE((1.00087707567816,1.00061365578608,1.))
REPRESENTATION_ITEM('')
);
#283=(
BOUNDED_CURVE()
B_SPLINE_CURVE(2,(#35805,#35806,#35807),.UNSPECIFIED.,.F.,.F.)
B_SPLINE_CURVE_WITH_KNOTS((3,3),(0.,0.0168038693768179),.UNSPECIFIED.)
CURVE()
GEOMETRIC_REPRESENTATION_ITEM()
RATIONAL_B_SPLINE_CURVE((1.,1.00061365578613,1.00087707567823))
REPRESENTATION_ITEM('')
);
#284=(
BOUNDED_CURVE()
B_SPLINE_CURVE(2,(#35812,#35813,#35814),.UNSPECIFIED.,.F.,.F.)
B_SPLINE_CURVE_WITH_KNOTS((3,3),(0.0420809670913823,0.0588848364681992),
 .UNSPECIFIED.)
CURVE()
GEOMETRIC_REPRESENTATION_ITEM()
RATIONAL_B_SPLINE_CURVE((1.00087707567815,1.00061365578607,1.))
REPRESENTATION_ITEM('')
);
#285=(
BOUNDED_CURVE()
B_SPLINE_CURVE(2,(#35819,#35820,#35821),.UNSPECIFIED.,.F.,.F.)
B_SPLINE_CURVE_WITH_KNOTS((3,3),(0.,0.0168038693768011),.UNSPECIFIED.)
CURVE()
GEOMETRIC_REPRESENTATION_ITEM()
RATIONAL_B_SPLINE_CURVE((1.,1.00061365578643,1.00087707567867))
REPRESENTATION_ITEM('')
);
#286=(
BOUNDED_CURVE()
B_SPLINE_CURVE(2,(#35826,#35827,#35828),.UNSPECIFIED.,.F.,.F.)
B_SPLINE_CURVE_WITH_KNOTS((3,3),(0.0420809670914,0.0588848364681992),
 .UNSPECIFIED.)
CURVE()
GEOMETRIC_REPRESENTATION_ITEM()
RATIONAL_B_SPLINE_CURVE((1.00087707567851,1.00061365578632,1.))
REPRESENTATION_ITEM('')
);
#287=(
BOUNDED_CURVE()
B_SPLINE_CURVE(2,(#35833,#35834,#35835),.UNSPECIFIED.,.F.,.F.)
B_SPLINE_CURVE_WITH_KNOTS((3,3),(0.,0.016803869376813),.UNSPECIFIED.)
CURVE()
GEOMETRIC_REPRESENTATION_ITEM()
RATIONAL_B_SPLINE_CURVE((1.,1.00061365578622,1.00087707567836))
REPRESENTATION_ITEM('')
);
#288=(
BOUNDED_CURVE()
B_SPLINE_CURVE(2,(#35840,#35841,#35842),.UNSPECIFIED.,.F.,.F.)
B_SPLINE_CURVE_WITH_KNOTS((3,3),(0.0420809670913641,0.0588848364681993),
 .UNSPECIFIED.)
CURVE()
GEOMETRIC_REPRESENTATION_ITEM()
RATIONAL_B_SPLINE_CURVE((1.0008770756778,1.00061365578582,1.))
REPRESENTATION_ITEM('')
);
#289=(
BOUNDED_CURVE()
B_SPLINE_CURVE(2,(#35847,#35848,#35849),.UNSPECIFIED.,.F.,.F.)
B_SPLINE_CURVE_WITH_KNOTS((3,3),(0.,0.0168038693768258),.UNSPECIFIED.)
CURVE()
GEOMETRIC_REPRESENTATION_ITEM()
RATIONAL_B_SPLINE_CURVE((1.,1.00061365578608,1.00087707567816))
REPRESENTATION_ITEM('')
);
#290=(
BOUNDED_CURVE()
B_SPLINE_CURVE(2,(#35854,#35855,#35856),.UNSPECIFIED.,.F.,.F.)
B_SPLINE_CURVE_WITH_KNOTS((3,3),(0.0420809670913328,0.0588848364681992),
 .UNSPECIFIED.)
CURVE()
GEOMETRIC_REPRESENTATION_ITEM()
RATIONAL_B_SPLINE_CURVE((1.00087707567803,1.00061365578599,1.))
REPRESENTATION_ITEM('')
);
#291=(
BOUNDED_CURVE()
B_SPLINE_CURVE(2,(#35861,#35862,#35863),.UNSPECIFIED.,.F.,.F.)
B_SPLINE_CURVE_WITH_KNOTS((3,3),(0.,0.016803869376812),.UNSPECIFIED.)
CURVE()
GEOMETRIC_REPRESENTATION_ITEM()
RATIONAL_B_SPLINE_CURVE((1.,1.00061365578602,1.00087707567807))
REPRESENTATION_ITEM('')
);
#292=(
BOUNDED_CURVE()
B_SPLINE_CURVE(2,(#35868,#35869,#35870),.UNSPECIFIED.,.F.,.F.)
B_SPLINE_CURVE_WITH_KNOTS((3,3),(0.0420809670913778,0.0588848364681992),
 .UNSPECIFIED.)
CURVE()
GEOMETRIC_REPRESENTATION_ITEM()
RATIONAL_B_SPLINE_CURVE((1.0008770756785,1.00061365578631,1.))
REPRESENTATION_ITEM('')
);
#293=(
BOUNDED_CURVE()
B_SPLINE_CURVE(2,(#35875,#35876,#35877),.UNSPECIFIED.,.F.,.F.)
B_SPLINE_CURVE_WITH_KNOTS((3,3),(0.,0.0168038693768374),.UNSPECIFIED.)
CURVE()
GEOMETRIC_REPRESENTATION_ITEM()
RATIONAL_B_SPLINE_CURVE((1.,1.00061365578616,1.00087707567828))
REPRESENTATION_ITEM('')
);
#294=(
BOUNDED_CURVE()
B_SPLINE_CURVE(2,(#35882,#35883,#35884),.UNSPECIFIED.,.F.,.F.)
B_SPLINE_CURVE_WITH_KNOTS((3,3),(0.0420809670913638,0.0588848364681993),
 .UNSPECIFIED.)
CURVE()
GEOMETRIC_REPRESENTATION_ITEM()
RATIONAL_B_SPLINE_CURVE((1.00087707567787,1.00061365578588,1.))
REPRESENTATION_ITEM('')
);
#295=(
BOUNDED_CURVE()
B_SPLINE_CURVE(2,(#35889,#35890,#35891),.UNSPECIFIED.,.F.,.F.)
B_SPLINE_CURVE_WITH_KNOTS((3,3),(0.,0.0168038693768215),.UNSPECIFIED.)
CURVE()
GEOMETRIC_REPRESENTATION_ITEM()
RATIONAL_B_SPLINE_CURVE((1.,1.00061365578602,1.00087707567808))
REPRESENTATION_ITEM('')
);
#296=(
BOUNDED_CURVE()
B_SPLINE_CURVE(2,(#35896,#35897,#35898),.UNSPECIFIED.,.F.,.F.)
B_SPLINE_CURVE_WITH_KNOTS((3,3),(0.0420809670913305,0.0588848364681993),
 .UNSPECIFIED.)
CURVE()
GEOMETRIC_REPRESENTATION_ITEM()
RATIONAL_B_SPLINE_CURVE((1.00087707567765,1.00061365578572,1.))
REPRESENTATION_ITEM('')
);
#297=(
BOUNDED_CURVE()
B_SPLINE_CURVE(2,(#35903,#35904,#35905),.UNSPECIFIED.,.F.,.F.)
B_SPLINE_CURVE_WITH_KNOTS((3,3),(0.,0.0168038693768224),.UNSPECIFIED.)
CURVE()
GEOMETRIC_REPRESENTATION_ITEM()
RATIONAL_B_SPLINE_CURVE((1.,1.00061365578599,1.00087707567803))
REPRESENTATION_ITEM('')
);
#298=(
BOUNDED_CURVE()
B_SPLINE_CURVE(2,(#35910,#35911,#35912),.UNSPECIFIED.,.F.,.F.)
B_SPLINE_CURVE_WITH_KNOTS((3,3),(0.0420809670913736,0.0588848364681993),
 .UNSPECIFIED.)
CURVE()
GEOMETRIC_REPRESENTATION_ITEM()
RATIONAL_B_SPLINE_CURVE((1.00087707567727,1.00061365578546,1.))
REPRESENTATION_ITEM('')
);
#299=(
BOUNDED_CURVE()
B_SPLINE_CURVE(2,(#35917,#35918,#35919),.UNSPECIFIED.,.F.,.F.)
B_SPLINE_CURVE_WITH_KNOTS((3,3),(0.,0.0168038693768305),.UNSPECIFIED.)
CURVE()
GEOMETRIC_REPRESENTATION_ITEM()
RATIONAL_B_SPLINE_CURVE((1.,1.00061365578611,1.00087707567821))
REPRESENTATION_ITEM('')
);
#300=(
BOUNDED_CURVE()
B_SPLINE_CURVE(2,(#35924,#35925,#35926),.UNSPECIFIED.,.F.,.F.)
B_SPLINE_CURVE_WITH_KNOTS((3,3),(0.042080967091357,0.0588848364681993),
 .UNSPECIFIED.)
CURVE()
GEOMETRIC_REPRESENTATION_ITEM()
RATIONAL_B_SPLINE_CURVE((1.00087707567817,1.00061365578609,1.))
REPRESENTATION_ITEM('')
);
#301=(
BOUNDED_CURVE()
B_SPLINE_CURVE(2,(#35931,#35932,#35933),.UNSPECIFIED.,.F.,.F.)
B_SPLINE_CURVE_WITH_KNOTS((3,3),(0.,0.0168038693768215),.UNSPECIFIED.)
CURVE()
GEOMETRIC_REPRESENTATION_ITEM()
RATIONAL_B_SPLINE_CURVE((1.,1.00061365578616,1.00087707567828))
REPRESENTATION_ITEM('')
);
#302=(
BOUNDED_CURVE()
B_SPLINE_CURVE(2,(#35938,#35939,#35940),.UNSPECIFIED.,.F.,.F.)
B_SPLINE_CURVE_WITH_KNOTS((3,3),(0.04208096709137,0.0588848364681993),
 .UNSPECIFIED.)
CURVE()
GEOMETRIC_REPRESENTATION_ITEM()
RATIONAL_B_SPLINE_CURVE((1.00087707567792,1.00061365578591,1.))
REPRESENTATION_ITEM('')
);
#303=(
BOUNDED_CURVE()
B_SPLINE_CURVE(2,(#35945,#35946,#35947),.UNSPECIFIED.,.F.,.F.)
B_SPLINE_CURVE_WITH_KNOTS((3,3),(0.,0.0168038693768075),.UNSPECIFIED.)
CURVE()
GEOMETRIC_REPRESENTATION_ITEM()
RATIONAL_B_SPLINE_CURVE((1.,1.00061365578628,1.00087707567845))
REPRESENTATION_ITEM('')
);
#304=(
BOUNDED_CURVE()
B_SPLINE_CURVE(2,(#35952,#35953,#35954),.UNSPECIFIED.,.F.,.F.)
B_SPLINE_CURVE_WITH_KNOTS((3,3),(0.0420809670913788,0.0588848364681993),
 .UNSPECIFIED.)
CURVE()
GEOMETRIC_REPRESENTATION_ITEM()
RATIONAL_B_SPLINE_CURVE((1.00087707567806,1.00061365578601,1.))
REPRESENTATION_ITEM('')
);
#305=(
BOUNDED_CURVE()
B_SPLINE_CURVE(2,(#35959,#35960,#35961),.UNSPECIFIED.,.F.,.F.)
B_SPLINE_CURVE_WITH_KNOTS((3,3),(0.,0.0168038693768069),.UNSPECIFIED.)
CURVE()
GEOMETRIC_REPRESENTATION_ITEM()
RATIONAL_B_SPLINE_CURVE((1.,1.00061365578667,1.000877075679))
REPRESENTATION_ITEM('')
);
#306=(
BOUNDED_CURVE()
B_SPLINE_CURVE(2,(#35966,#35967,#35968),.UNSPECIFIED.,.F.,.F.)
B_SPLINE_CURVE_WITH_KNOTS((3,3),(0.0420809670913639,0.0588848364681993),
 .UNSPECIFIED.)
CURVE()
GEOMETRIC_REPRESENTATION_ITEM()
RATIONAL_B_SPLINE_CURVE((1.00087707567811,1.00061365578604,1.))
REPRESENTATION_ITEM('')
);
#307=(
BOUNDED_CURVE()
B_SPLINE_CURVE(2,(#35973,#35974,#35975),.UNSPECIFIED.,.F.,.F.)
B_SPLINE_CURVE_WITH_KNOTS((3,3),(0.,0.0168038693768441),.UNSPECIFIED.)
CURVE()
GEOMETRIC_REPRESENTATION_ITEM()
RATIONAL_B_SPLINE_CURVE((1.,1.00061365578625,1.0008770756784))
REPRESENTATION_ITEM('')
);
#308=(
BOUNDED_CURVE()
B_SPLINE_CURVE(2,(#35980,#35981,#35982),.UNSPECIFIED.,.F.,.F.)
B_SPLINE_CURVE_WITH_KNOTS((3,3),(0.0420809670913765,0.0588848364681993),
 .UNSPECIFIED.)
CURVE()
GEOMETRIC_REPRESENTATION_ITEM()
RATIONAL_B_SPLINE_CURVE((1.00087707567789,1.00061365578589,1.))
REPRESENTATION_ITEM('')
);
#309=(
BOUNDED_CURVE()
B_SPLINE_CURVE(2,(#35987,#35988,#35989),.UNSPECIFIED.,.F.,.F.)
B_SPLINE_CURVE_WITH_KNOTS((3,3),(0.,0.016803869376822),.UNSPECIFIED.)
CURVE()
GEOMETRIC_REPRESENTATION_ITEM()
RATIONAL_B_SPLINE_CURVE((1.,1.00061365578656,1.00087707567884))
REPRESENTATION_ITEM('')
);
#310=(
BOUNDED_CURVE()
B_SPLINE_CURVE(2,(#35994,#35995,#35996),.UNSPECIFIED.,.F.,.F.)
B_SPLINE_CURVE_WITH_KNOTS((3,3),(0.0420809670913437,0.0588848364681993),
 .UNSPECIFIED.)
CURVE()
GEOMETRIC_REPRESENTATION_ITEM()
RATIONAL_B_SPLINE_CURVE((1.00087707567775,1.00061365578579,1.))
REPRESENTATION_ITEM('')
);
#311=(
BOUNDED_CURVE()
B_SPLINE_CURVE(2,(#36001,#36002,#36003),.UNSPECIFIED.,.F.,.F.)
B_SPLINE_CURVE_WITH_KNOTS((3,3),(0.,0.0168038693768237),.UNSPECIFIED.)
CURVE()
GEOMETRIC_REPRESENTATION_ITEM()
RATIONAL_B_SPLINE_CURVE((1.,1.00061365578586,1.00087707567785))
REPRESENTATION_ITEM('')
);
#312=(
BOUNDED_CURVE()
B_SPLINE_CURVE(2,(#36008,#36009,#36010),.UNSPECIFIED.,.F.,.F.)
B_SPLINE_CURVE_WITH_KNOTS((3,3),(0.0420809670913633,0.0588848364681993),
 .UNSPECIFIED.)
CURVE()
GEOMETRIC_REPRESENTATION_ITEM()
RATIONAL_B_SPLINE_CURVE((1.00087707567797,1.00061365578594,1.))
REPRESENTATION_ITEM('')
);
#313=(
BOUNDED_CURVE()
B_SPLINE_CURVE(2,(#36015,#36016,#36017),.UNSPECIFIED.,.F.,.F.)
B_SPLINE_CURVE_WITH_KNOTS((3,3),(0.,0.0168038693768391),.UNSPECIFIED.)
CURVE()
GEOMETRIC_REPRESENTATION_ITEM()
RATIONAL_B_SPLINE_CURVE((1.,1.00061365578625,1.0008770756784))
REPRESENTATION_ITEM('')
);
#314=(
BOUNDED_CURVE()
B_SPLINE_CURVE(2,(#36022,#36023,#36024),.UNSPECIFIED.,.F.,.F.)
B_SPLINE_CURVE_WITH_KNOTS((3,3),(0.0420809670913792,0.0588848364681992),
 .UNSPECIFIED.)
CURVE()
GEOMETRIC_REPRESENTATION_ITEM()
RATIONAL_B_SPLINE_CURVE((1.00087707567848,1.0006136557863,1.))
REPRESENTATION_ITEM('')
);
#315=(
BOUNDED_CURVE()
B_SPLINE_CURVE(2,(#36029,#36030,#36031),.UNSPECIFIED.,.F.,.F.)
B_SPLINE_CURVE_WITH_KNOTS((3,3),(0.,0.0168038693768203),.UNSPECIFIED.)
CURVE()
GEOMETRIC_REPRESENTATION_ITEM()
RATIONAL_B_SPLINE_CURVE((1.,1.00061365578598,1.00087707567802))
REPRESENTATION_ITEM('')
);
#316=(
BOUNDED_CURVE()
B_SPLINE_CURVE(2,(#36036,#36037,#36038),.UNSPECIFIED.,.F.,.F.)
B_SPLINE_CURVE_WITH_KNOTS((3,3),(0.0420809670913809,0.0588848364681992),
 .UNSPECIFIED.)
CURVE()
GEOMETRIC_REPRESENTATION_ITEM()
RATIONAL_B_SPLINE_CURVE((1.00087707567876,1.0006136557865,1.))
REPRESENTATION_ITEM('')
);
#317=(
BOUNDED_CURVE()
B_SPLINE_CURVE(2,(#36043,#36044,#36045),.UNSPECIFIED.,.F.,.F.)
B_SPLINE_CURVE_WITH_KNOTS((3,3),(0.,0.016803869376822),.UNSPECIFIED.)
CURVE()
GEOMETRIC_REPRESENTATION_ITEM()
RATIONAL_B_SPLINE_CURVE((1.,1.00061365578629,1.00087707567847))
REPRESENTATION_ITEM('')
);
#318=(
BOUNDED_CURVE()
B_SPLINE_CURVE(2,(#36050,#36051,#36052),.UNSPECIFIED.,.F.,.F.)
B_SPLINE_CURVE_WITH_KNOTS((3,3),(0.0420809670913693,0.0588848364681992),
 .UNSPECIFIED.)
CURVE()
GEOMETRIC_REPRESENTATION_ITEM()
RATIONAL_B_SPLINE_CURVE((1.00087707567787,1.00061365578588,1.))
REPRESENTATION_ITEM('')
);
#319=(
BOUNDED_CURVE()
B_SPLINE_CURVE(2,(#36057,#36058,#36059),.UNSPECIFIED.,.F.,.F.)
B_SPLINE_CURVE_WITH_KNOTS((3,3),(0.,0.0168038693768241),.UNSPECIFIED.)
CURVE()
GEOMETRIC_REPRESENTATION_ITEM()
RATIONAL_B_SPLINE_CURVE((1.,1.00061365578674,1.00087707567911))
REPRESENTATION_ITEM('')
);
#320=(
BOUNDED_CURVE()
B_SPLINE_CURVE(2,(#36064,#36065,#36066),.UNSPECIFIED.,.F.,.F.)
B_SPLINE_CURVE_WITH_KNOTS((3,3),(0.0420809670913706,0.0588848364681992),
 .UNSPECIFIED.)
CURVE()
GEOMETRIC_REPRESENTATION_ITEM()
RATIONAL_B_SPLINE_CURVE((1.00087707567803,1.00061365578598,1.))
REPRESENTATION_ITEM('')
);
#321=(
BOUNDED_CURVE()
B_SPLINE_CURVE(2,(#36071,#36072,#36073),.UNSPECIFIED.,.F.,.F.)
B_SPLINE_CURVE_WITH_KNOTS((3,3),(0.,0.0168038693768352),.UNSPECIFIED.)
CURVE()
GEOMETRIC_REPRESENTATION_ITEM()
RATIONAL_B_SPLINE_CURVE((1.,1.00061365578544,1.00087707567725))
REPRESENTATION_ITEM('')
);
#322=(
BOUNDED_CURVE()
B_SPLINE_CURVE(2,(#36078,#36079,#36080),.UNSPECIFIED.,.F.,.F.)
B_SPLINE_CURVE_WITH_KNOTS((3,3),(0.0420809670913822,0.0588848364681993),
 .UNSPECIFIED.)
CURVE()
GEOMETRIC_REPRESENTATION_ITEM()
RATIONAL_B_SPLINE_CURVE((1.00087707567791,1.00061365578591,1.))
REPRESENTATION_ITEM('')
);
#323=(
BOUNDED_CURVE()
B_SPLINE_CURVE(2,(#36085,#36086,#36087),.UNSPECIFIED.,.F.,.F.)
B_SPLINE_CURVE_WITH_KNOTS((3,3),(0.,0.0168038693768391),.UNSPECIFIED.)
CURVE()
GEOMETRIC_REPRESENTATION_ITEM()
RATIONAL_B_SPLINE_CURVE((1.,1.00061365578625,1.0008770756784))
REPRESENTATION_ITEM('')
);
#324=(
BOUNDED_CURVE()
B_SPLINE_CURVE(2,(#36092,#36093,#36094),.UNSPECIFIED.,.F.,.F.)
B_SPLINE_CURVE_WITH_KNOTS((3,3),(0.0420809670913788,0.0588848364681992),
 .UNSPECIFIED.)
CURVE()
GEOMETRIC_REPRESENTATION_ITEM()
RATIONAL_B_SPLINE_CURVE((1.00087707567811,1.00061365578604,1.))
REPRESENTATION_ITEM('')
);
#325=(
BOUNDED_CURVE()
B_SPLINE_CURVE(2,(#36099,#36100,#36101),.UNSPECIFIED.,.F.,.F.)
B_SPLINE_CURVE_WITH_KNOTS((3,3),(0.,0.0168038693768716),.UNSPECIFIED.)
CURVE()
GEOMETRIC_REPRESENTATION_ITEM()
RATIONAL_B_SPLINE_CURVE((1.,1.00061365578607,1.00087707567815))
REPRESENTATION_ITEM('')
);
#326=(
BOUNDED_CURVE()
B_SPLINE_CURVE(2,(#36106,#36107,#36108),.UNSPECIFIED.,.F.,.F.)
B_SPLINE_CURVE_WITH_KNOTS((3,3),(0.0420809670913493,0.0588848364681993),
 .UNSPECIFIED.)
CURVE()
GEOMETRIC_REPRESENTATION_ITEM()
RATIONAL_B_SPLINE_CURVE((1.00087707567838,1.00061365578623,1.))
REPRESENTATION_ITEM('')
);
#327=(
BOUNDED_CURVE()
B_SPLINE_CURVE(2,(#36113,#36114,#36115),.UNSPECIFIED.,.F.,.F.)
B_SPLINE_CURVE_WITH_KNOTS((3,3),(0.,0.0168038693768289),.UNSPECIFIED.)
CURVE()
GEOMETRIC_REPRESENTATION_ITEM()
RATIONAL_B_SPLINE_CURVE((1.,1.00061365578616,1.00087707567828))
REPRESENTATION_ITEM('')
);
#328=(
BOUNDED_CURVE()
B_SPLINE_CURVE(2,(#36120,#36121,#36122),.UNSPECIFIED.,.F.,.F.)
B_SPLINE_CURVE_WITH_KNOTS((3,3),(0.0420809670913749,0.0588848364681992),
 .UNSPECIFIED.)
CURVE()
GEOMETRIC_REPRESENTATION_ITEM()
RATIONAL_B_SPLINE_CURVE((1.00087707567811,1.00061365578604,1.))
REPRESENTATION_ITEM('')
);
#329=(
BOUNDED_CURVE()
B_SPLINE_CURVE(2,(#36127,#36128,#36129),.UNSPECIFIED.,.F.,.F.)
B_SPLINE_CURVE_WITH_KNOTS((3,3),(0.,0.0168038693768264),.UNSPECIFIED.)
CURVE()
GEOMETRIC_REPRESENTATION_ITEM()
RATIONAL_B_SPLINE_CURVE((1.,1.00061365578613,1.00087707567823))
REPRESENTATION_ITEM('')
);
#330=(
BOUNDED_CURVE()
B_SPLINE_CURVE(2,(#36134,#36135,#36136),.UNSPECIFIED.,.F.,.F.)
B_SPLINE_CURVE_WITH_KNOTS((3,3),(0.0420809670913744,0.0588848364681992),
 .UNSPECIFIED.)
CURVE()
GEOMETRIC_REPRESENTATION_ITEM()
RATIONAL_B_SPLINE_CURVE((1.00087707567875,1.00061365578649,1.))
REPRESENTATION_ITEM('')
);
#331=(
BOUNDED_CURVE()
B_SPLINE_CURVE(2,(#36141,#36142,#36143),.UNSPECIFIED.,.F.,.F.)
B_SPLINE_CURVE_WITH_KNOTS((3,3),(0.,0.0168038693768507),.UNSPECIFIED.)
CURVE()
GEOMETRIC_REPRESENTATION_ITEM()
RATIONAL_B_SPLINE_CURVE((1.,1.00061365578591,1.00087707567792))
REPRESENTATION_ITEM('')
);
#332=(
BOUNDED_CURVE()
B_SPLINE_CURVE(2,(#36148,#36149,#36150),.UNSPECIFIED.,.F.,.F.)
B_SPLINE_CURVE_WITH_KNOTS((3,3),(0.0420809670913786,0.0588848364681993),
 .UNSPECIFIED.)
CURVE()
GEOMETRIC_REPRESENTATION_ITEM()
RATIONAL_B_SPLINE_CURVE((1.00087707567801,1.00061365578597,1.))
REPRESENTATION_ITEM('')
);
#333=(
BOUNDED_CURVE()
B_SPLINE_CURVE(2,(#36155,#36156,#36157),.UNSPECIFIED.,.F.,.F.)
B_SPLINE_CURVE_WITH_KNOTS((3,3),(0.,0.0168038693768258),.UNSPECIFIED.)
CURVE()
GEOMETRIC_REPRESENTATION_ITEM()
RATIONAL_B_SPLINE_CURVE((1.,1.00061365578592,1.00087707567793))
REPRESENTATION_ITEM('')
);
#334=(
BOUNDED_CURVE()
B_SPLINE_CURVE(2,(#36162,#36163,#36164),.UNSPECIFIED.,.F.,.F.)
B_SPLINE_CURVE_WITH_KNOTS((3,3),(0.0420809670913652,0.0588848364681993),
 .UNSPECIFIED.)
CURVE()
GEOMETRIC_REPRESENTATION_ITEM()
RATIONAL_B_SPLINE_CURVE((1.00087707567844,1.00061365578627,1.))
REPRESENTATION_ITEM('')
);
#335=(
BOUNDED_CURVE()
B_SPLINE_CURVE(2,(#36169,#36170,#36171),.UNSPECIFIED.,.F.,.F.)
B_SPLINE_CURVE_WITH_KNOTS((3,3),(0.,0.0168038693768152),.UNSPECIFIED.)
CURVE()
GEOMETRIC_REPRESENTATION_ITEM()
RATIONAL_B_SPLINE_CURVE((1.,1.00061365578615,1.00087707567826))
REPRESENTATION_ITEM('')
);
#336=(
BOUNDED_CURVE()
B_SPLINE_CURVE(2,(#37921,#37922,#37923),.UNSPECIFIED.,.F.,.F.)
B_SPLINE_CURVE_WITH_KNOTS((3,3),(0.0395243267589975,0.0757709160687003),
 .UNSPECIFIED.)
CURVE()
GEOMETRIC_REPRESENTATION_ITEM()
RATIONAL_B_SPLINE_CURVE((1.00144403367688,1.00138415709391,1.))
REPRESENTATION_ITEM('')
);
#337=(
BOUNDED_CURVE()
B_SPLINE_CURVE(2,(#37927,#37928,#37929),.UNSPECIFIED.,.F.,.F.)
B_SPLINE_CURVE_WITH_KNOTS((3,3),(0.,0.0368264807252771),.UNSPECIFIED.)
CURVE()
GEOMETRIC_REPRESENTATION_ITEM()
RATIONAL_B_SPLINE_CURVE((1.,1.00108727860041,1.00085032920655))
REPRESENTATION_ITEM('')
);
#338=(
BOUNDED_CURVE()
B_SPLINE_CURVE(2,(#37933,#37934,#37935),.UNSPECIFIED.,.F.,.F.)
B_SPLINE_CURVE_WITH_KNOTS((3,3),(0.,0.0362465893096916),.UNSPECIFIED.)
CURVE()
GEOMETRIC_REPRESENTATION_ITEM()
RATIONAL_B_SPLINE_CURVE((1.,1.00138415709372,1.00144403367668))
REPRESENTATION_ITEM('')
);
#339=(
BOUNDED_CURVE()
B_SPLINE_CURVE(2,(#37938,#37939,#37940),.UNSPECIFIED.,.F.,.F.)
B_SPLINE_CURVE_WITH_KNOTS((3,3),(0.023647462726297,0.0604739434515668),
 .UNSPECIFIED.)
CURVE()
GEOMETRIC_REPRESENTATION_ITEM()
RATIONAL_B_SPLINE_CURVE((1.00085032920655,1.0010872786004,1.))
REPRESENTATION_ITEM('')
);
#340=(
BOUNDED_CURVE()
B_SPLINE_CURVE(2,(#37944,#37945,#37946),.UNSPECIFIED.,.F.,.F.)
B_SPLINE_CURVE_WITH_KNOTS((3,3),(0.0395243267590134,0.0757709160687001),
 .UNSPECIFIED.)
CURVE()
GEOMETRIC_REPRESENTATION_ITEM()
RATIONAL_B_SPLINE_CURVE((1.00144403367689,1.00138415709393,1.))
REPRESENTATION_ITEM('')
);
#341=(
BOUNDED_CURVE()
B_SPLINE_CURVE(2,(#37950,#37951,#37952),.UNSPECIFIED.,.F.,.F.)
B_SPLINE_CURVE_WITH_KNOTS((3,3),(0.,0.036826480725251),.UNSPECIFIED.)
CURVE()
GEOMETRIC_REPRESENTATION_ITEM()
RATIONAL_B_SPLINE_CURVE((1.,1.00108727860024,1.00085032920643))
REPRESENTATION_ITEM('')
);
#342=(
BOUNDED_CURVE()
B_SPLINE_CURVE(2,(#37956,#37957,#37958),.UNSPECIFIED.,.F.,.F.)
B_SPLINE_CURVE_WITH_KNOTS((3,3),(0.,0.0362465893097029),.UNSPECIFIED.)
CURVE()
GEOMETRIC_REPRESENTATION_ITEM()
RATIONAL_B_SPLINE_CURVE((1.,1.00138415709418,1.00144403367715))
REPRESENTATION_ITEM('')
);
#343=(
BOUNDED_CURVE()
B_SPLINE_CURVE(2,(#37961,#37962,#37963),.UNSPECIFIED.,.F.,.F.)
B_SPLINE_CURVE_WITH_KNOTS((3,3),(0.0236474627262938,0.060473943451567),
 .UNSPECIFIED.)
CURVE()
GEOMETRIC_REPRESENTATION_ITEM()
RATIONAL_B_SPLINE_CURVE((1.00085032920586,1.00108727859952,1.))
REPRESENTATION_ITEM('')
);
#344=(
BOUNDED_CURVE()
B_SPLINE_CURVE(2,(#37967,#37968,#37969),.UNSPECIFIED.,.F.,.F.)
B_SPLINE_CURVE_WITH_KNOTS((3,3),(0.0395243267590093,0.0757709160687003),
 .UNSPECIFIED.)
CURVE()
GEOMETRIC_REPRESENTATION_ITEM()
RATIONAL_B_SPLINE_CURVE((1.00144403367677,1.00138415709381,1.))
REPRESENTATION_ITEM('')
);
#345=(
BOUNDED_CURVE()
B_SPLINE_CURVE(2,(#37973,#37974,#37975),.UNSPECIFIED.,.F.,.F.)
B_SPLINE_CURVE_WITH_KNOTS((3,3),(0.,0.0368264807252646),.UNSPECIFIED.)
CURVE()
GEOMETRIC_REPRESENTATION_ITEM()
RATIONAL_B_SPLINE_CURVE((1.,1.00108727859976,1.00085032920605))
REPRESENTATION_ITEM('')
);
#346=(
BOUNDED_CURVE()
B_SPLINE_CURVE(2,(#37979,#37980,#37981),.UNSPECIFIED.,.F.,.F.)
B_SPLINE_CURVE_WITH_KNOTS((3,3),(0.,0.0362465893097049),.UNSPECIFIED.)
CURVE()
GEOMETRIC_REPRESENTATION_ITEM()
RATIONAL_B_SPLINE_CURVE((1.,1.0013841570941,1.00144403367707))
REPRESENTATION_ITEM('')
);
#347=(
BOUNDED_CURVE()
B_SPLINE_CURVE(2,(#37984,#37985,#37986),.UNSPECIFIED.,.F.,.F.)
B_SPLINE_CURVE_WITH_KNOTS((3,3),(0.0236474627263067,0.0604739434515669),
 .UNSPECIFIED.)
CURVE()
GEOMETRIC_REPRESENTATION_ITEM()
RATIONAL_B_SPLINE_CURVE((1.00085032920563,1.00108727859922,1.))
REPRESENTATION_ITEM('')
);
#348=(
BOUNDED_CURVE()
B_SPLINE_CURVE(2,(#37990,#37991,#37992),.UNSPECIFIED.,.F.,.F.)
B_SPLINE_CURVE_WITH_KNOTS((3,3),(0.0395243267589975,0.0757709160687003),
 .UNSPECIFIED.)
CURVE()
GEOMETRIC_REPRESENTATION_ITEM()
RATIONAL_B_SPLINE_CURVE((1.00144403367688,1.00138415709391,1.))
REPRESENTATION_ITEM('')
);
#349=(
BOUNDED_CURVE()
B_SPLINE_CURVE(2,(#37996,#37997,#37998),.UNSPECIFIED.,.F.,.F.)
B_SPLINE_CURVE_WITH_KNOTS((3,3),(0.,0.0368264807252771),.UNSPECIFIED.)
CURVE()
GEOMETRIC_REPRESENTATION_ITEM()
RATIONAL_B_SPLINE_CURVE((1.,1.00108727860041,1.00085032920655))
REPRESENTATION_ITEM('')
);
#350=(
BOUNDED_CURVE()
B_SPLINE_CURVE(2,(#38002,#38003,#38004),.UNSPECIFIED.,.F.,.F.)
B_SPLINE_CURVE_WITH_KNOTS((3,3),(0.,0.0362465893096841),.UNSPECIFIED.)
CURVE()
GEOMETRIC_REPRESENTATION_ITEM()
RATIONAL_B_SPLINE_CURVE((1.,1.00138415709402,1.00144403367699))
REPRESENTATION_ITEM('')
);
#351=(
BOUNDED_CURVE()
B_SPLINE_CURVE(2,(#38007,#38008,#38009),.UNSPECIFIED.,.F.,.F.)
B_SPLINE_CURVE_WITH_KNOTS((3,3),(0.0236474627263223,0.0604739434515668),
 .UNSPECIFIED.)
CURVE()
GEOMETRIC_REPRESENTATION_ITEM()
RATIONAL_B_SPLINE_CURVE((1.00085032920605,1.00108727859975,1.))
REPRESENTATION_ITEM('')
);
#352=(
BOUNDED_CURVE()
B_SPLINE_CURVE(2,(#38013,#38014,#38015),.UNSPECIFIED.,.F.,.F.)
B_SPLINE_CURVE_WITH_KNOTS((3,3),(0.0395243267590166,0.0757709160687002),
 .UNSPECIFIED.)
CURVE()
GEOMETRIC_REPRESENTATION_ITEM()
RATIONAL_B_SPLINE_CURVE((1.00144403367685,1.00138415709388,1.))
REPRESENTATION_ITEM('')
);
#353=(
BOUNDED_CURVE()
B_SPLINE_CURVE(2,(#38019,#38020,#38021),.UNSPECIFIED.,.F.,.F.)
B_SPLINE_CURVE_WITH_KNOTS((3,3),(0.,0.0368264807252521),.UNSPECIFIED.)
CURVE()
GEOMETRIC_REPRESENTATION_ITEM()
RATIONAL_B_SPLINE_CURVE((1.,1.00108727859996,1.0008503292062))
REPRESENTATION_ITEM('')
);
#354=(
BOUNDED_CURVE()
B_SPLINE_CURVE(2,(#38025,#38026,#38027),.UNSPECIFIED.,.F.,.F.)
B_SPLINE_CURVE_WITH_KNOTS((3,3),(0.,0.0362465893096854),.UNSPECIFIED.)
CURVE()
GEOMETRIC_REPRESENTATION_ITEM()
RATIONAL_B_SPLINE_CURVE((1.,1.0013841570938,1.00144403367676))
REPRESENTATION_ITEM('')
);
#355=(
BOUNDED_CURVE()
B_SPLINE_CURVE(2,(#38030,#38031,#38032),.UNSPECIFIED.,.F.,.F.)
B_SPLINE_CURVE_WITH_KNOTS((3,3),(0.0236474627263314,0.0604739434515669),
 .UNSPECIFIED.)
CURVE()
GEOMETRIC_REPRESENTATION_ITEM()
RATIONAL_B_SPLINE_CURVE((1.00085032920606,1.00108727859977,1.))
REPRESENTATION_ITEM('')
);
#356=(
BOUNDED_CURVE()
B_SPLINE_CURVE(2,(#38036,#38037,#38038),.UNSPECIFIED.,.F.,.F.)
B_SPLINE_CURVE_WITH_KNOTS((3,3),(0.0395243267589997,0.0757709160687002),
 .UNSPECIFIED.)
CURVE()
GEOMETRIC_REPRESENTATION_ITEM()
RATIONAL_B_SPLINE_CURVE((1.00144403367698,1.00138415709401,1.))
REPRESENTATION_ITEM('')
);
#357=(
BOUNDED_CURVE()
B_SPLINE_CURVE(2,(#38042,#38043,#38044),.UNSPECIFIED.,.F.,.F.)
B_SPLINE_CURVE_WITH_KNOTS((3,3),(0.,0.0368264807252651),.UNSPECIFIED.)
CURVE()
GEOMETRIC_REPRESENTATION_ITEM()
RATIONAL_B_SPLINE_CURVE((1.,1.00108727860044,1.00085032920658))
REPRESENTATION_ITEM('')
);
#358=(
BOUNDED_CURVE()
B_SPLINE_CURVE(2,(#38048,#38049,#38050),.UNSPECIFIED.,.F.,.F.)
B_SPLINE_CURVE_WITH_KNOTS((3,3),(0.,0.0362465893096843),.UNSPECIFIED.)
CURVE()
GEOMETRIC_REPRESENTATION_ITEM()
RATIONAL_B_SPLINE_CURVE((1.,1.00138415709419,1.00144403367717))
REPRESENTATION_ITEM('')
);
#359=(
BOUNDED_CURVE()
B_SPLINE_CURVE(2,(#38053,#38054,#38055),.UNSPECIFIED.,.F.,.F.)
B_SPLINE_CURVE_WITH_KNOTS((3,3),(0.0236474627263023,0.060473943451567),
 .UNSPECIFIED.)
CURVE()
GEOMETRIC_REPRESENTATION_ITEM()
RATIONAL_B_SPLINE_CURVE((1.00085032920674,1.00108727860064,1.))
REPRESENTATION_ITEM('')
);
#360=(
BOUNDED_CURVE()
B_SPLINE_CURVE(2,(#38059,#38060,#38061),.UNSPECIFIED.,.F.,.F.)
B_SPLINE_CURVE_WITH_KNOTS((3,3),(0.0395243267590068,0.0757709160687003),
 .UNSPECIFIED.)
CURVE()
GEOMETRIC_REPRESENTATION_ITEM()
RATIONAL_B_SPLINE_CURVE((1.00144403367694,1.00138415709397,1.))
REPRESENTATION_ITEM('')
);
#361=(
BOUNDED_CURVE()
B_SPLINE_CURVE(2,(#38065,#38066,#38067),.UNSPECIFIED.,.F.,.F.)
B_SPLINE_CURVE_WITH_KNOTS((3,3),(0.,0.0368264807252612),.UNSPECIFIED.)
CURVE()
GEOMETRIC_REPRESENTATION_ITEM()
RATIONAL_B_SPLINE_CURVE((1.,1.00108727859988,1.00085032920614))
REPRESENTATION_ITEM('')
);
#362=(
BOUNDED_CURVE()
B_SPLINE_CURVE(2,(#38071,#38072,#38073),.UNSPECIFIED.,.F.,.F.)
B_SPLINE_CURVE_WITH_KNOTS((3,3),(0.,0.0362465893096925),.UNSPECIFIED.)
CURVE()
GEOMETRIC_REPRESENTATION_ITEM()
RATIONAL_B_SPLINE_CURVE((1.,1.00138415709391,1.00144403367687))
REPRESENTATION_ITEM('')
);
#363=(
BOUNDED_CURVE()
B_SPLINE_CURVE(2,(#38076,#38077,#38078),.UNSPECIFIED.,.F.,.F.)
B_SPLINE_CURVE_WITH_KNOTS((3,3),(0.0236474627263132,0.0604739434515669),
 .UNSPECIFIED.)
CURVE()
GEOMETRIC_REPRESENTATION_ITEM()
RATIONAL_B_SPLINE_CURVE((1.0008503292066,1.00108727860046,1.))
REPRESENTATION_ITEM('')
);
#364=(
BOUNDED_CURVE()
B_SPLINE_CURVE(2,(#38082,#38083,#38084),.UNSPECIFIED.,.F.,.F.)
B_SPLINE_CURVE_WITH_KNOTS((3,3),(0.039524326759018,0.0757709160687002),
 .UNSPECIFIED.)
CURVE()
GEOMETRIC_REPRESENTATION_ITEM()
RATIONAL_B_SPLINE_CURVE((1.00144403367702,1.00138415709405,1.))
REPRESENTATION_ITEM('')
);
#365=(
BOUNDED_CURVE()
B_SPLINE_CURVE(2,(#38088,#38089,#38090),.UNSPECIFIED.,.F.,.F.)
B_SPLINE_CURVE_WITH_KNOTS((3,3),(0.,0.0368264807252612),.UNSPECIFIED.)
CURVE()
GEOMETRIC_REPRESENTATION_ITEM()
RATIONAL_B_SPLINE_CURVE((1.,1.00108727860027,1.00085032920645))
REPRESENTATION_ITEM('')
);
#366=(
BOUNDED_CURVE()
B_SPLINE_CURVE(2,(#38094,#38095,#38096),.UNSPECIFIED.,.F.,.F.)
B_SPLINE_CURVE_WITH_KNOTS((3,3),(0.,0.0362465893096848),.UNSPECIFIED.)
CURVE()
GEOMETRIC_REPRESENTATION_ITEM()
RATIONAL_B_SPLINE_CURVE((1.,1.00138415709428,1.00144403367727))
REPRESENTATION_ITEM('')
);
#367=(
BOUNDED_CURVE()
B_SPLINE_CURVE(2,(#38099,#38100,#38101),.UNSPECIFIED.,.F.,.F.)
B_SPLINE_CURVE_WITH_KNOTS((3,3),(0.0236474627263229,0.060473943451567),
 .UNSPECIFIED.)
CURVE()
GEOMETRIC_REPRESENTATION_ITEM()
RATIONAL_B_SPLINE_CURVE((1.00085032920677,1.00108727860068,1.))
REPRESENTATION_ITEM('')
);
#368=(
BOUNDED_CURVE()
B_SPLINE_CURVE(2,(#38105,#38106,#38107),.UNSPECIFIED.,.F.,.F.)
B_SPLINE_CURVE_WITH_KNOTS((3,3),(0.0395243267590142,0.0757709160687002),
 .UNSPECIFIED.)
CURVE()
GEOMETRIC_REPRESENTATION_ITEM()
RATIONAL_B_SPLINE_CURVE((1.00144403367701,1.00138415709404,1.))
REPRESENTATION_ITEM('')
);
#369=(
BOUNDED_CURVE()
B_SPLINE_CURVE(2,(#38111,#38112,#38113),.UNSPECIFIED.,.F.,.F.)
B_SPLINE_CURVE_WITH_KNOTS((3,3),(0.,0.0368264807252614),.UNSPECIFIED.)
CURVE()
GEOMETRIC_REPRESENTATION_ITEM()
RATIONAL_B_SPLINE_CURVE((1.,1.00108727860056,1.00085032920667))
REPRESENTATION_ITEM('')
);
#370=(
BOUNDED_CURVE()
B_SPLINE_CURVE(2,(#38117,#38118,#38119),.UNSPECIFIED.,.F.,.F.)
B_SPLINE_CURVE_WITH_KNOTS((3,3),(0.,0.0362465893096775),.UNSPECIFIED.)
CURVE()
GEOMETRIC_REPRESENTATION_ITEM()
RATIONAL_B_SPLINE_CURVE((1.,1.00138415709412,1.0014440336771))
REPRESENTATION_ITEM('')
);
#371=(
BOUNDED_CURVE()
B_SPLINE_CURVE(2,(#38122,#38123,#38124),.UNSPECIFIED.,.F.,.F.)
B_SPLINE_CURVE_WITH_KNOTS((3,3),(0.023647462726333,0.060473943451567),
 .UNSPECIFIED.)
CURVE()
GEOMETRIC_REPRESENTATION_ITEM()
RATIONAL_B_SPLINE_CURVE((1.00085032920627,1.00108727860004,1.))
REPRESENTATION_ITEM('')
);
#372=(
BOUNDED_CURVE()
B_SPLINE_CURVE(2,(#38128,#38129,#38130),.UNSPECIFIED.,.F.,.F.)
B_SPLINE_CURVE_WITH_KNOTS((3,3),(0.0395243267590017,0.0757709160687002),
 .UNSPECIFIED.)
CURVE()
GEOMETRIC_REPRESENTATION_ITEM()
RATIONAL_B_SPLINE_CURVE((1.00144403367696,1.00138415709399,1.))
REPRESENTATION_ITEM('')
);
#373=(
BOUNDED_CURVE()
B_SPLINE_CURVE(2,(#38134,#38135,#38136),.UNSPECIFIED.,.F.,.F.)
B_SPLINE_CURVE_WITH_KNOTS((3,3),(0.,0.0368264807252428),.UNSPECIFIED.)
CURVE()
GEOMETRIC_REPRESENTATION_ITEM()
RATIONAL_B_SPLINE_CURVE((1.,1.00108727860007,1.0008503292063))
REPRESENTATION_ITEM('')
);
#374=(
BOUNDED_CURVE()
B_SPLINE_CURVE(2,(#38140,#38141,#38142),.UNSPECIFIED.,.F.,.F.)
B_SPLINE_CURVE_WITH_KNOTS((3,3),(0.,0.036246589309685),.UNSPECIFIED.)
CURVE()
GEOMETRIC_REPRESENTATION_ITEM()
RATIONAL_B_SPLINE_CURVE((1.,1.00138415709379,1.00144403367676))
REPRESENTATION_ITEM('')
);
#375=(
BOUNDED_CURVE()
B_SPLINE_CURVE(2,(#38145,#38146,#38147),.UNSPECIFIED.,.F.,.F.)
B_SPLINE_CURVE_WITH_KNOTS((3,3),(0.0236474627262961,0.060473943451567),
 .UNSPECIFIED.)
CURVE()
GEOMETRIC_REPRESENTATION_ITEM()
RATIONAL_B_SPLINE_CURVE((1.00085032920624,1.0010872786,1.))
REPRESENTATION_ITEM('')
);
#376=(
BOUNDED_CURVE()
B_SPLINE_CURVE(2,(#38151,#38152,#38153),.UNSPECIFIED.,.F.,.F.)
B_SPLINE_CURVE_WITH_KNOTS((3,3),(0.0395243267590158,0.0757709160687002),
 .UNSPECIFIED.)
CURVE()
GEOMETRIC_REPRESENTATION_ITEM()
RATIONAL_B_SPLINE_CURVE((1.0014440336769,1.00138415709393,1.))
REPRESENTATION_ITEM('')
);
#377=(
BOUNDED_CURVE()
B_SPLINE_CURVE(2,(#38157,#38158,#38159),.UNSPECIFIED.,.F.,.F.)
B_SPLINE_CURVE_WITH_KNOTS((3,3),(0.,0.0368264807252534),.UNSPECIFIED.)
CURVE()
GEOMETRIC_REPRESENTATION_ITEM()
RATIONAL_B_SPLINE_CURVE((1.,1.00108727860033,1.00085032920649))
REPRESENTATION_ITEM('')
);
#378=(
BOUNDED_CURVE()
B_SPLINE_CURVE(2,(#38163,#38164,#38165),.UNSPECIFIED.,.F.,.F.)
B_SPLINE_CURVE_WITH_KNOTS((3,3),(0.,0.0362465893096853),.UNSPECIFIED.)
CURVE()
GEOMETRIC_REPRESENTATION_ITEM()
RATIONAL_B_SPLINE_CURVE((1.,1.00138415709412,1.0014440336771))
REPRESENTATION_ITEM('')
);
#379=(
BOUNDED_CURVE()
B_SPLINE_CURVE(2,(#38168,#38169,#38170),.UNSPECIFIED.,.F.,.F.)
B_SPLINE_CURVE_WITH_KNOTS((3,3),(0.0236474627263147,0.060473943451567),
 .UNSPECIFIED.)
CURVE()
GEOMETRIC_REPRESENTATION_ITEM()
RATIONAL_B_SPLINE_CURVE((1.00085032920646,1.00108727860028,1.))
REPRESENTATION_ITEM('')
);
#380=(
BOUNDED_CURVE()
B_SPLINE_CURVE(2,(#38174,#38175,#38176),.UNSPECIFIED.,.F.,.F.)
B_SPLINE_CURVE_WITH_KNOTS((3,3),(0.0395243267590156,0.0757709160687002),
 .UNSPECIFIED.)
CURVE()
GEOMETRIC_REPRESENTATION_ITEM()
RATIONAL_B_SPLINE_CURVE((1.00144403367684,1.00138415709387,1.))
REPRESENTATION_ITEM('')
);
#381=(
BOUNDED_CURVE()
B_SPLINE_CURVE(2,(#38180,#38181,#38182),.UNSPECIFIED.,.F.,.F.)
B_SPLINE_CURVE_WITH_KNOTS((3,3),(0.,0.0368264807252693),.UNSPECIFIED.)
CURVE()
GEOMETRIC_REPRESENTATION_ITEM()
RATIONAL_B_SPLINE_CURVE((1.,1.00108727859986,1.00085032920613))
REPRESENTATION_ITEM('')
);
#382=(
BOUNDED_CURVE()
B_SPLINE_CURVE(2,(#38186,#38187,#38188),.UNSPECIFIED.,.F.,.F.)
B_SPLINE_CURVE_WITH_KNOTS((3,3),(0.,0.0362465893096901),.UNSPECIFIED.)
CURVE()
GEOMETRIC_REPRESENTATION_ITEM()
RATIONAL_B_SPLINE_CURVE((1.,1.00138415709395,1.00144403367692))
REPRESENTATION_ITEM('')
);
#383=(
BOUNDED_CURVE()
B_SPLINE_CURVE(2,(#38191,#38192,#38193),.UNSPECIFIED.,.F.,.F.)
B_SPLINE_CURVE_WITH_KNOTS((3,3),(0.0236474627263255,0.0604739434515669),
 .UNSPECIFIED.)
CURVE()
GEOMETRIC_REPRESENTATION_ITEM()
RATIONAL_B_SPLINE_CURVE((1.0008503292064,1.00108727860021,1.))
REPRESENTATION_ITEM('')
);
#384=(
BOUNDED_CURVE()
B_SPLINE_CURVE(2,(#38197,#38198,#38199),.UNSPECIFIED.,.F.,.F.)
B_SPLINE_CURVE_WITH_KNOTS((3,3),(0.0395243267590232,0.0757709160687003),
 .UNSPECIFIED.)
CURVE()
GEOMETRIC_REPRESENTATION_ITEM()
RATIONAL_B_SPLINE_CURVE((1.0014440336771,1.00138415709412,1.))
REPRESENTATION_ITEM('')
);
#385=(
BOUNDED_CURVE()
B_SPLINE_CURVE(2,(#38203,#38204,#38205),.UNSPECIFIED.,.F.,.F.)
B_SPLINE_CURVE_WITH_KNOTS((3,3),(0.,0.0368264807252497),.UNSPECIFIED.)
CURVE()
GEOMETRIC_REPRESENTATION_ITEM()
RATIONAL_B_SPLINE_CURVE((1.,1.00108727859942,1.00085032920579))
REPRESENTATION_ITEM('')
);
#386=(
BOUNDED_CURVE()
B_SPLINE_CURVE(2,(#38209,#38210,#38211),.UNSPECIFIED.,.F.,.F.)
B_SPLINE_CURVE_WITH_KNOTS((3,3),(0.,0.0362465893096849),.UNSPECIFIED.)
CURVE()
GEOMETRIC_REPRESENTATION_ITEM()
RATIONAL_B_SPLINE_CURVE((1.,1.00138415709363,1.00144403367659))
REPRESENTATION_ITEM('')
);
#387=(
BOUNDED_CURVE()
B_SPLINE_CURVE(2,(#38214,#38215,#38216),.UNSPECIFIED.,.F.,.F.)
B_SPLINE_CURVE_WITH_KNOTS((3,3),(0.0236474627263162,0.060473943451567),
 .UNSPECIFIED.)
CURVE()
GEOMETRIC_REPRESENTATION_ITEM()
RATIONAL_B_SPLINE_CURVE((1.00085032920633,1.00108727860012,1.))
REPRESENTATION_ITEM('')
);
#388=(
BOUNDED_CURVE()
B_SPLINE_CURVE(2,(#38220,#38221,#38222),.UNSPECIFIED.,.F.,.F.)
B_SPLINE_CURVE_WITH_KNOTS((3,3),(0.0395243267590082,0.0757709160687002),
 .UNSPECIFIED.)
CURVE()
GEOMETRIC_REPRESENTATION_ITEM()
RATIONAL_B_SPLINE_CURVE((1.00144403367716,1.00138415709418,1.))
REPRESENTATION_ITEM('')
);
#389=(
BOUNDED_CURVE()
B_SPLINE_CURVE(2,(#38226,#38227,#38228),.UNSPECIFIED.,.F.,.F.)
B_SPLINE_CURVE_WITH_KNOTS((3,3),(0.,0.0368264807252609),.UNSPECIFIED.)
CURVE()
GEOMETRIC_REPRESENTATION_ITEM()
RATIONAL_B_SPLINE_CURVE((1.,1.00108727859987,1.00085032920614))
REPRESENTATION_ITEM('')
);
#390=(
BOUNDED_CURVE()
B_SPLINE_CURVE(2,(#38232,#38233,#38234),.UNSPECIFIED.,.F.,.F.)
B_SPLINE_CURVE_WITH_KNOTS((3,3),(0.,0.0362465893096812),.UNSPECIFIED.)
CURVE()
GEOMETRIC_REPRESENTATION_ITEM()
RATIONAL_B_SPLINE_CURVE((1.,1.0013841570937,1.00144403367666))
REPRESENTATION_ITEM('')
);
#391=(
BOUNDED_CURVE()
B_SPLINE_CURVE(2,(#38237,#38238,#38239),.UNSPECIFIED.,.F.,.F.)
B_SPLINE_CURVE_WITH_KNOTS((3,3),(0.0236474627263107,0.0604739434515669),
 .UNSPECIFIED.)
CURVE()
GEOMETRIC_REPRESENTATION_ITEM()
RATIONAL_B_SPLINE_CURVE((1.00085032920669,1.00108727860058,1.))
REPRESENTATION_ITEM('')
);
#392=(
BOUNDED_CURVE()
B_SPLINE_CURVE(2,(#38243,#38244,#38245),.UNSPECIFIED.,.F.,.F.)
B_SPLINE_CURVE_WITH_KNOTS((3,3),(0.0395243267589996,0.0757709160687002),
 .UNSPECIFIED.)
CURVE()
GEOMETRIC_REPRESENTATION_ITEM()
RATIONAL_B_SPLINE_CURVE((1.00144403367705,1.00138415709408,1.))
REPRESENTATION_ITEM('')
);
#393=(
BOUNDED_CURVE()
B_SPLINE_CURVE(2,(#38249,#38250,#38251),.UNSPECIFIED.,.F.,.F.)
B_SPLINE_CURVE_WITH_KNOTS((3,3),(0.,0.0368264807252541),.UNSPECIFIED.)
CURVE()
GEOMETRIC_REPRESENTATION_ITEM()
RATIONAL_B_SPLINE_CURVE((1.,1.00108727860017,1.00085032920637))
REPRESENTATION_ITEM('')
);
#394=(
BOUNDED_CURVE()
B_SPLINE_CURVE(2,(#38255,#38256,#38257),.UNSPECIFIED.,.F.,.F.)
B_SPLINE_CURVE_WITH_KNOTS((3,3),(0.,0.0362465893096801),.UNSPECIFIED.)
CURVE()
GEOMETRIC_REPRESENTATION_ITEM()
RATIONAL_B_SPLINE_CURVE((1.,1.00138415709414,1.00144403367712))
REPRESENTATION_ITEM('')
);
#395=(
BOUNDED_CURVE()
B_SPLINE_CURVE(2,(#38260,#38261,#38262),.UNSPECIFIED.,.F.,.F.)
B_SPLINE_CURVE_WITH_KNOTS((3,3),(0.0236474627263037,0.060473943451567),
 .UNSPECIFIED.)
CURVE()
GEOMETRIC_REPRESENTATION_ITEM()
RATIONAL_B_SPLINE_CURVE((1.00085032920654,1.00108727860038,1.))
REPRESENTATION_ITEM('')
);
#396=(
BOUNDED_CURVE()
B_SPLINE_CURVE(2,(#38266,#38267,#38268),.UNSPECIFIED.,.F.,.F.)
B_SPLINE_CURVE_WITH_KNOTS((3,3),(0.0395243267590246,0.0757709160687002),
 .UNSPECIFIED.)
CURVE()
GEOMETRIC_REPRESENTATION_ITEM()
RATIONAL_B_SPLINE_CURVE((1.00144403367709,1.00138415709411,1.))
REPRESENTATION_ITEM('')
);
#397=(
BOUNDED_CURVE()
B_SPLINE_CURVE(2,(#38272,#38273,#38274),.UNSPECIFIED.,.F.,.F.)
B_SPLINE_CURVE_WITH_KNOTS((3,3),(0.,0.0368264807252722),.UNSPECIFIED.)
CURVE()
GEOMETRIC_REPRESENTATION_ITEM()
RATIONAL_B_SPLINE_CURVE((1.,1.00108727859999,1.00085032920623))
REPRESENTATION_ITEM('')
);
#398=(
BOUNDED_CURVE()
B_SPLINE_CURVE(2,(#38278,#38279,#38280),.UNSPECIFIED.,.F.,.F.)
B_SPLINE_CURVE_WITH_KNOTS((3,3),(0.,0.036246589309683),.UNSPECIFIED.)
CURVE()
GEOMETRIC_REPRESENTATION_ITEM()
RATIONAL_B_SPLINE_CURVE((1.,1.00138415709414,1.00144403367712))
REPRESENTATION_ITEM('')
);
#399=(
BOUNDED_CURVE()
B_SPLINE_CURVE(2,(#38283,#38284,#38285),.UNSPECIFIED.,.F.,.F.)
B_SPLINE_CURVE_WITH_KNOTS((3,3),(0.0236474627263149,0.060473943451567),
 .UNSPECIFIED.)
CURVE()
GEOMETRIC_REPRESENTATION_ITEM()
RATIONAL_B_SPLINE_CURVE((1.00085032920643,1.00108727860025,1.))
REPRESENTATION_ITEM('')
);
#400=(
BOUNDED_CURVE()
B_SPLINE_CURVE(2,(#38289,#38290,#38291),.UNSPECIFIED.,.F.,.F.)
B_SPLINE_CURVE_WITH_KNOTS((3,3),(0.0395243267590166,0.0757709160687002),
 .UNSPECIFIED.)
CURVE()
GEOMETRIC_REPRESENTATION_ITEM()
RATIONAL_B_SPLINE_CURVE((1.00144403367727,1.00138415709429,1.))
REPRESENTATION_ITEM('')
);
#401=(
BOUNDED_CURVE()
B_SPLINE_CURVE(2,(#38295,#38296,#38297),.UNSPECIFIED.,.F.,.F.)
B_SPLINE_CURVE_WITH_KNOTS((3,3),(0.,0.0368264807252481),.UNSPECIFIED.)
CURVE()
GEOMETRIC_REPRESENTATION_ITEM()
RATIONAL_B_SPLINE_CURVE((1.,1.00108727859946,1.00085032920581))
REPRESENTATION_ITEM('')
);
#402=(
BOUNDED_CURVE()
B_SPLINE_CURVE(2,(#38301,#38302,#38303),.UNSPECIFIED.,.F.,.F.)
B_SPLINE_CURVE_WITH_KNOTS((3,3),(0.,0.0362465893096797),.UNSPECIFIED.)
CURVE()
GEOMETRIC_REPRESENTATION_ITEM()
RATIONAL_B_SPLINE_CURVE((1.,1.00138415709394,1.00144403367691))
REPRESENTATION_ITEM('')
);
#403=(
BOUNDED_CURVE()
B_SPLINE_CURVE(2,(#38306,#38307,#38308),.UNSPECIFIED.,.F.,.F.)
B_SPLINE_CURVE_WITH_KNOTS((3,3),(0.0236474627263141,0.0604739434515669),
 .UNSPECIFIED.)
CURVE()
GEOMETRIC_REPRESENTATION_ITEM()
RATIONAL_B_SPLINE_CURVE((1.00085032920622,1.00108727859997,1.))
REPRESENTATION_ITEM('')
);
#404=(
BOUNDED_CURVE()
B_SPLINE_CURVE(2,(#38312,#38313,#38314),.UNSPECIFIED.,.F.,.F.)
B_SPLINE_CURVE_WITH_KNOTS((3,3),(0.0395243267590075,0.0757709160687003),
 .UNSPECIFIED.)
CURVE()
GEOMETRIC_REPRESENTATION_ITEM()
RATIONAL_B_SPLINE_CURVE((1.00144403367703,1.00138415709406,1.))
REPRESENTATION_ITEM('')
);
#405=(
BOUNDED_CURVE()
B_SPLINE_CURVE(2,(#38318,#38319,#38320),.UNSPECIFIED.,.F.,.F.)
B_SPLINE_CURVE_WITH_KNOTS((3,3),(0.,0.0368264807252487),.UNSPECIFIED.)
CURVE()
GEOMETRIC_REPRESENTATION_ITEM()
RATIONAL_B_SPLINE_CURVE((1.,1.00108727859994,1.00085032920619))
REPRESENTATION_ITEM('')
);
#406=(
BOUNDED_CURVE()
B_SPLINE_CURVE(2,(#38324,#38325,#38326),.UNSPECIFIED.,.F.,.F.)
B_SPLINE_CURVE_WITH_KNOTS((3,3),(0.,0.0362465893096912),.UNSPECIFIED.)
CURVE()
GEOMETRIC_REPRESENTATION_ITEM()
RATIONAL_B_SPLINE_CURVE((1.,1.00138415709428,1.00144403367727))
REPRESENTATION_ITEM('')
);
#407=(
BOUNDED_CURVE()
B_SPLINE_CURVE(2,(#38329,#38330,#38331),.UNSPECIFIED.,.F.,.F.)
B_SPLINE_CURVE_WITH_KNOTS((3,3),(0.0236474627263162,0.0604739434515669),
 .UNSPECIFIED.)
CURVE()
GEOMETRIC_REPRESENTATION_ITEM()
RATIONAL_B_SPLINE_CURVE((1.00085032920654,1.00108727860038,1.))
REPRESENTATION_ITEM('')
);
#408=(
BOUNDED_CURVE()
B_SPLINE_CURVE(2,(#38335,#38336,#38337),.UNSPECIFIED.,.F.,.F.)
B_SPLINE_CURVE_WITH_KNOTS((3,3),(0.0395243267590164,0.0757709160687002),
 .UNSPECIFIED.)
CURVE()
GEOMETRIC_REPRESENTATION_ITEM()
RATIONAL_B_SPLINE_CURVE((1.0014440336769,1.00138415709393,1.))
REPRESENTATION_ITEM('')
);
#409=(
BOUNDED_CURVE()
B_SPLINE_CURVE(2,(#38341,#38342,#38343),.UNSPECIFIED.,.F.,.F.)
B_SPLINE_CURVE_WITH_KNOTS((3,3),(0.,0.0368264807252535),.UNSPECIFIED.)
CURVE()
GEOMETRIC_REPRESENTATION_ITEM()
RATIONAL_B_SPLINE_CURVE((1.,1.00108727860031,1.00085032920648))
REPRESENTATION_ITEM('')
);
#410=(
BOUNDED_CURVE()
B_SPLINE_CURVE(2,(#38347,#38348,#38349),.UNSPECIFIED.,.F.,.F.)
B_SPLINE_CURVE_WITH_KNOTS((3,3),(0.,0.0362465893096775),.UNSPECIFIED.)
CURVE()
GEOMETRIC_REPRESENTATION_ITEM()
RATIONAL_B_SPLINE_CURVE((1.,1.00138415709412,1.0014440336771))
REPRESENTATION_ITEM('')
);
#411=(
BOUNDED_CURVE()
B_SPLINE_CURVE(2,(#38352,#38353,#38354),.UNSPECIFIED.,.F.,.F.)
B_SPLINE_CURVE_WITH_KNOTS((3,3),(0.023647462726333,0.060473943451567),
 .UNSPECIFIED.)
CURVE()
GEOMETRIC_REPRESENTATION_ITEM()
RATIONAL_B_SPLINE_CURVE((1.00085032920627,1.00108727860004,1.))
REPRESENTATION_ITEM('')
);
#412=(
BOUNDED_CURVE()
B_SPLINE_CURVE(2,(#38358,#38359,#38360),.UNSPECIFIED.,.F.,.F.)
B_SPLINE_CURVE_WITH_KNOTS((3,3),(0.03952432675902,0.0757709160687003),
 .UNSPECIFIED.)
CURVE()
GEOMETRIC_REPRESENTATION_ITEM()
RATIONAL_B_SPLINE_CURVE((1.00144403367664,1.00138415709369,1.))
REPRESENTATION_ITEM('')
);
#413=(
BOUNDED_CURVE()
B_SPLINE_CURVE(2,(#38364,#38365,#38366),.UNSPECIFIED.,.F.,.F.)
B_SPLINE_CURVE_WITH_KNOTS((3,3),(0.,0.0368264807252641),.UNSPECIFIED.)
CURVE()
GEOMETRIC_REPRESENTATION_ITEM()
RATIONAL_B_SPLINE_CURVE((1.,1.00108727860008,1.0008503292063))
REPRESENTATION_ITEM('')
);
#414=(
BOUNDED_CURVE()
B_SPLINE_CURVE(2,(#38370,#38371,#38372),.UNSPECIFIED.,.F.,.F.)
B_SPLINE_CURVE_WITH_KNOTS((3,3),(0.,0.0362465893096867),.UNSPECIFIED.)
CURVE()
GEOMETRIC_REPRESENTATION_ITEM()
RATIONAL_B_SPLINE_CURVE((1.,1.00138415709384,1.0014440336768))
REPRESENTATION_ITEM('')
);
#415=(
BOUNDED_CURVE()
B_SPLINE_CURVE(2,(#38375,#38376,#38377),.UNSPECIFIED.,.F.,.F.)
B_SPLINE_CURVE_WITH_KNOTS((3,3),(0.0236474627263162,0.060473943451567),
 .UNSPECIFIED.)
CURVE()
GEOMETRIC_REPRESENTATION_ITEM()
RATIONAL_B_SPLINE_CURVE((1.00085032920569,1.0010872785993,1.))
REPRESENTATION_ITEM('')
);
#416=(
BOUNDED_CURVE()
B_SPLINE_CURVE(2,(#38381,#38382,#38383),.UNSPECIFIED.,.F.,.F.)
B_SPLINE_CURVE_WITH_KNOTS((3,3),(0.0395243267590018,0.0757709160687002),
 .UNSPECIFIED.)
CURVE()
GEOMETRIC_REPRESENTATION_ITEM()
RATIONAL_B_SPLINE_CURVE((1.00144403367701,1.00138415709404,1.))
REPRESENTATION_ITEM('')
);
#417=(
BOUNDED_CURVE()
B_SPLINE_CURVE(2,(#38387,#38388,#38389),.UNSPECIFIED.,.F.,.F.)
B_SPLINE_CURVE_WITH_KNOTS((3,3),(0.,0.0368264807252595),.UNSPECIFIED.)
CURVE()
GEOMETRIC_REPRESENTATION_ITEM()
RATIONAL_B_SPLINE_CURVE((1.,1.00108727860035,1.00085032920651))
REPRESENTATION_ITEM('')
);
#418=(
BOUNDED_CURVE()
B_SPLINE_CURVE(2,(#38393,#38394,#38395),.UNSPECIFIED.,.F.,.F.)
B_SPLINE_CURVE_WITH_KNOTS((3,3),(0.,0.0362465893096985),.UNSPECIFIED.)
CURVE()
GEOMETRIC_REPRESENTATION_ITEM()
RATIONAL_B_SPLINE_CURVE((1.,1.00138415709386,1.00144403367682))
REPRESENTATION_ITEM('')
);
#419=(
BOUNDED_CURVE()
B_SPLINE_CURVE(2,(#38398,#38399,#38400),.UNSPECIFIED.,.F.,.F.)
B_SPLINE_CURVE_WITH_KNOTS((3,3),(0.0236474627262938,0.060473943451567),
 .UNSPECIFIED.)
CURVE()
GEOMETRIC_REPRESENTATION_ITEM()
RATIONAL_B_SPLINE_CURVE((1.00085032920587,1.00108727859953,1.))
REPRESENTATION_ITEM('')
);
#420=(
BOUNDED_CURVE()
B_SPLINE_CURVE(2,(#38404,#38405,#38406),.UNSPECIFIED.,.F.,.F.)
B_SPLINE_CURVE_WITH_KNOTS((3,3),(0.0395243267590063,0.0757709160687004),
 .UNSPECIFIED.)
CURVE()
GEOMETRIC_REPRESENTATION_ITEM()
RATIONAL_B_SPLINE_CURVE((1.00144403367682,1.00138415709386,1.))
REPRESENTATION_ITEM('')
);
#421=(
BOUNDED_CURVE()
B_SPLINE_CURVE(2,(#38410,#38411,#38412),.UNSPECIFIED.,.F.,.F.)
B_SPLINE_CURVE_WITH_KNOTS((3,3),(0.,0.0368264807252569),.UNSPECIFIED.)
CURVE()
GEOMETRIC_REPRESENTATION_ITEM()
RATIONAL_B_SPLINE_CURVE((1.,1.00108727859996,1.00085032920621))
REPRESENTATION_ITEM('')
);
#422=(
BOUNDED_CURVE()
B_SPLINE_CURVE(2,(#38416,#38417,#38418),.UNSPECIFIED.,.F.,.F.)
B_SPLINE_CURVE_WITH_KNOTS((3,3),(0.,0.0362465893096971),.UNSPECIFIED.)
CURVE()
GEOMETRIC_REPRESENTATION_ITEM()
RATIONAL_B_SPLINE_CURVE((1.,1.00138415709408,1.00144403367705))
REPRESENTATION_ITEM('')
);
#423=(
BOUNDED_CURVE()
B_SPLINE_CURVE(2,(#38421,#38422,#38423),.UNSPECIFIED.,.F.,.F.)
B_SPLINE_CURVE_WITH_KNOTS((3,3),(0.0236474627263185,0.0604739434515669),
 .UNSPECIFIED.)
CURVE()
GEOMETRIC_REPRESENTATION_ITEM()
RATIONAL_B_SPLINE_CURVE((1.00085032920632,1.0010872786001,1.))
REPRESENTATION_ITEM('')
);
#424=(
BOUNDED_CURVE()
B_SPLINE_CURVE(2,(#38427,#38428,#38429),.UNSPECIFIED.,.F.,.F.)
B_SPLINE_CURVE_WITH_KNOTS((3,3),(0.0395243267590211,0.0757709160687003),
 .UNSPECIFIED.)
CURVE()
GEOMETRIC_REPRESENTATION_ITEM()
RATIONAL_B_SPLINE_CURVE((1.00144403367694,1.00138415709397,1.))
REPRESENTATION_ITEM('')
);
#425=(
BOUNDED_CURVE()
B_SPLINE_CURVE(2,(#38433,#38434,#38435),.UNSPECIFIED.,.F.,.F.)
B_SPLINE_CURVE_WITH_KNOTS((3,3),(0.,0.0368264807252641),.UNSPECIFIED.)
CURVE()
GEOMETRIC_REPRESENTATION_ITEM()
RATIONAL_B_SPLINE_CURVE((1.,1.00108727860008,1.0008503292063))
REPRESENTATION_ITEM('')
);
#426=(
BOUNDED_CURVE()
B_SPLINE_CURVE(2,(#38439,#38440,#38441),.UNSPECIFIED.,.F.,.F.)
B_SPLINE_CURVE_WITH_KNOTS((3,3),(0.,0.0362465893097037),.UNSPECIFIED.)
CURVE()
GEOMETRIC_REPRESENTATION_ITEM()
RATIONAL_B_SPLINE_CURVE((1.,1.00138415709397,1.00144403367693))
REPRESENTATION_ITEM('')
);
#427=(
BOUNDED_CURVE()
B_SPLINE_CURVE(2,(#38444,#38445,#38446),.UNSPECIFIED.,.F.,.F.)
B_SPLINE_CURVE_WITH_KNOTS((3,3),(0.023647462726311,0.0604739434515669),
 .UNSPECIFIED.)
CURVE()
GEOMETRIC_REPRESENTATION_ITEM()
RATIONAL_B_SPLINE_CURVE((1.00085032920618,1.00108727859993,1.))
REPRESENTATION_ITEM('')
);
#428=(
BOUNDED_CURVE()
B_SPLINE_CURVE(2,(#38450,#38451,#38452),.UNSPECIFIED.,.F.,.F.)
B_SPLINE_CURVE_WITH_KNOTS((3,3),(0.0395243267590132,0.0757709160687002),
 .UNSPECIFIED.)
CURVE()
GEOMETRIC_REPRESENTATION_ITEM()
RATIONAL_B_SPLINE_CURVE((1.00144403367714,1.00138415709416,1.))
REPRESENTATION_ITEM('')
);
#429=(
BOUNDED_CURVE()
B_SPLINE_CURVE(2,(#38456,#38457,#38458),.UNSPECIFIED.,.F.,.F.)
B_SPLINE_CURVE_WITH_KNOTS((3,3),(0.,0.0368264807252791),.UNSPECIFIED.)
CURVE()
GEOMETRIC_REPRESENTATION_ITEM()
RATIONAL_B_SPLINE_CURVE((1.,1.0010872786001,1.00085032920631))
REPRESENTATION_ITEM('')
);
#430=(
BOUNDED_CURVE()
B_SPLINE_CURVE(2,(#38462,#38463,#38464),.UNSPECIFIED.,.F.,.F.)
B_SPLINE_CURVE_WITH_KNOTS((3,3),(0.,0.0362465893096923),.UNSPECIFIED.)
CURVE()
GEOMETRIC_REPRESENTATION_ITEM()
RATIONAL_B_SPLINE_CURVE((1.,1.00138415709398,1.00144403367695))
REPRESENTATION_ITEM('')
);
#431=(
BOUNDED_CURVE()
B_SPLINE_CURVE(2,(#38467,#38468,#38469),.UNSPECIFIED.,.F.,.F.)
B_SPLINE_CURVE_WITH_KNOTS((3,3),(0.0236474627263034,0.060473943451567),
 .UNSPECIFIED.)
CURVE()
GEOMETRIC_REPRESENTATION_ITEM()
RATIONAL_B_SPLINE_CURVE((1.00085032920706,1.00108727860106,1.))
REPRESENTATION_ITEM('')
);
#432=SHAPE_REPRESENTATION_RELATIONSHIP('SRR','None',#38668,#446);
#433=SHAPE_REPRESENTATION_RELATIONSHIP('SRR','None',#38669,#447);
#434=SHAPE_REPRESENTATION_RELATIONSHIP('SRR','None',#38670,#448);
#435=SHAPE_REPRESENTATION_RELATIONSHIP('SRR','None',#38671,#449);
#436=SHAPE_REPRESENTATION_RELATIONSHIP('SRR','None',#38672,#450);
#437=SHAPE_REPRESENTATION_RELATIONSHIP('SRR','None',#38673,#451);
#438=SHAPE_REPRESENTATION_RELATIONSHIP('SRR','None',#38674,#452);
#439=SHAPE_REPRESENTATION_RELATIONSHIP('SRR','None',#38675,#453);
#440=SHAPE_REPRESENTATION_RELATIONSHIP('SRR','None',#38676,#454);
#441=SHAPE_REPRESENTATION_RELATIONSHIP('SRR','None',#38677,#455);
#442=SHAPE_REPRESENTATION_RELATIONSHIP('SRR','None',#38678,#456);
#443=SHAPE_REPRESENTATION_RELATIONSHIP('SRR','None',#38679,#457);
#444=SHAPE_REPRESENTATION_RELATIONSHIP('SRR','None',#38680,#458);
#445=SHAPE_REPRESENTATION_RELATIONSHIP('SRR','None',#38681,#459);
#446=ADVANCED_BREP_SHAPE_REPRESENTATION('',(#474),#38597);
#447=ADVANCED_BREP_SHAPE_REPRESENTATION('',(#475),#38598);
#448=ADVANCED_BREP_SHAPE_REPRESENTATION('',(#476),#38599);
#449=ADVANCED_BREP_SHAPE_REPRESENTATION('',(#477),#38600);
#450=ADVANCED_BREP_SHAPE_REPRESENTATION('',(#478),#38601);
#451=ADVANCED_BREP_SHAPE_REPRESENTATION('',(#479),#38602);
#452=ADVANCED_BREP_SHAPE_REPRESENTATION('',(#480),#38603);
#453=ADVANCED_BREP_SHAPE_REPRESENTATION('',(#481),#38604);
#454=ADVANCED_BREP_SHAPE_REPRESENTATION('',(#482),#38605);
#455=ADVANCED_BREP_SHAPE_REPRESENTATION('',(#483),#38606);
#456=ADVANCED_BREP_SHAPE_REPRESENTATION('',(#484),#38607);
#457=ADVANCED_BREP_SHAPE_REPRESENTATION('',(#485),#38608);
#458=ADVANCED_BREP_SHAPE_REPRESENTATION('',(#486),#38609);
#459=ADVANCED_BREP_SHAPE_REPRESENTATION('',(#487),#38610);
#460=STYLED_ITEM('',(#38857),#474);
#461=STYLED_ITEM('',(#38871),#475);
#462=STYLED_ITEM('',(#38878),#476);
#463=STYLED_ITEM('',(#38871),#477);
#464=STYLED_ITEM('',(#38871),#478);
#465=STYLED_ITEM('',(#38871),#479);
#466=STYLED_ITEM('',(#38885),#480);
#467=STYLED_ITEM('',(#38885),#481);
#468=STYLED_ITEM('',(#38857),#482);
#469=STYLED_ITEM('',(#38885),#483);
#470=STYLED_ITEM('',(#38864),#484);
#471=STYLED_ITEM('',(#38878),#485);
#472=STYLED_ITEM('',(#38885),#486);
#473=STYLED_ITEM('',(#38885),#487);
#474=MANIFOLD_SOLID_BREP('Foot',#16234);
#475=MANIFOLD_SOLID_BREP('Tube',#16235);
#476=MANIFOLD_SOLID_BREP('Rod',#16236);
#477=MANIFOLD_SOLID_BREP('Mirror plate',#16237);
#478=MANIFOLD_SOLID_BREP('Mirror',#16238);
#479=MANIFOLD_SOLID_BREP('Ring',#16239);
#480=MANIFOLD_SOLID_BREP('Set screw',#16240);
#481=MANIFOLD_SOLID_BREP('Set screw',#16241);
#482=MANIFOLD_SOLID_BREP('Bracket',#16242);
#483=MANIFOLD_SOLID_BREP('Adjuster',#16243);
#484=MANIFOLD_SOLID_BREP('Ball',#16244);
#485=MANIFOLD_SOLID_BREP('Spring',#16245);
#486=MANIFOLD_SOLID_BREP('Screw',#16246);
#487=MANIFOLD_SOLID_BREP('Thumb screw',#16247);
#488=TOROIDAL_SURFACE('',#16513,1.75,0.15);
#489=TOROIDAL_SURFACE('',#17387,0.2154,0.02);
#490=B_SPLINE_SURFACE_WITH_KNOTS('',3,3,((#22029,#22030,#22031,#22032,#22033,
#22034,#22035,#22036,#22037,#22038,#22039,#22040,#22041,#22042,#22043,#22044,
#22045,#22046,#22047,#22048,#22049,#22050),(#22051,#22052,#22053,#22054,
#22055,#22056,#22057,#22058,#22059,#22060,#22061,#22062,#22063,#22064,#22065,
#22066,#22067,#22068,#22069,#22070,#22071,#22072),(#22073,#22074,#22075,
#22076,#22077,#22078,#22079,#22080,#22081,#22082,#22083,#22084,#22085,#22086,
#22087,#22088,#22089,#22090,#22091,#22092,#22093,#22094),(#22095,#22096,
#22097,#22098,#22099,#22100,#22101,#22102,#22103,#22104,#22105,#22106,#22107,
#22108,#22109,#22110,#22111,#22112,#22113,#22114,#22115,#22116)),
 .UNSPECIFIED.,.F.,.T.,.F.,(4,4),(4,1,1,1,1,1,1,1,1,1,1,1,1,1,1,1,1,1,1,
4),(0.,1.),(0.,0.0885228467060966,0.177045693412193,0.221307116765241,0.26556854011829,
0.354091386824386,0.442614233530483,0.486875656883531,0.531137080236579,
0.619659926942676,0.708182773648772,0.752444197001821,0.796705620354869,
0.840967043707917,0.885228467060966,0.973751313767062,1.01801273712011,
1.06227416047316,1.15079700717926,1.23931985388535),.UNSPECIFIED.);
#491=B_SPLINE_SURFACE_WITH_KNOTS('',3,3,((#22409,#22410,#22411,#22412,#22413,
#22414,#22415,#22416,#22417,#22418,#22419,#22420,#22421,#22422,#22423,#22424,
#22425,#22426),(#22427,#22428,#22429,#22430,#22431,#22432,#22433,#22434,
#22435,#22436,#22437,#22438,#22439,#22440,#22441,#22442,#22443,#22444),
(#22445,#22446,#22447,#22448,#22449,#22450,#22451,#22452,#22453,#22454,
#22455,#22456,#22457,#22458,#22459,#22460,#22461,#22462),(#22463,#22464,
#22465,#22466,#22467,#22468,#22469,#22470,#22471,#22472,#22473,#22474,#22475,
#22476,#22477,#22478,#22479,#22480)),.UNSPECIFIED.,.F.,.T.,.F.,(4,4),(4,
1,1,1,1,1,1,1,1,1,1,1,1,1,1,4),(0.,1.),(0.,0.0883566653548034,0.176713330709607,
0.26506999606441,0.353426661419213,0.441783326774017,0.485961659451418,
0.53013999212882,0.706853322838427,0.751031655515829,0.79520998819323,0.883566653548034,
0.971923318902837,1.06027998425764,1.14863664961244,1.23699331496725),
 .UNSPECIFIED.);
#492=B_SPLINE_SURFACE_WITH_KNOTS('',3,3,((#23661,#23662,#23663,#23664,#23665,
#23666,#23667,#23668,#23669,#23670,#23671,#23672,#23673,#23674,#23675,#23676,
#23677,#23678,#23679,#23680,#23681,#23682,#23683,#23684,#23685,#23686,#23687,
#23688,#23689,#23690,#23691,#23692,#23693,#23694,#23695,#23696,#23697),
(#23698,#23699,#23700,#23701,#23702,#23703,#23704,#23705,#23706,#23707,
#23708,#23709,#23710,#23711,#23712,#23713,#23714,#23715,#23716,#23717,#23718,
#23719,#23720,#23721,#23722,#23723,#23724,#23725,#23726,#23727,#23728,#23729,
#23730,#23731,#23732,#23733,#23734),(#23735,#23736,#23737,#23738,#23739,
#23740,#23741,#23742,#23743,#23744,#23745,#23746,#23747,#23748,#23749,#23750,
#23751,#23752,#23753,#23754,#23755,#23756,#23757,#23758,#23759,#23760,#23761,
#23762,#23763,#23764,#23765,#23766,#23767,#23768,#23769,#23770,#23771),
(#23772,#23773,#23774,#23775,#23776,#23777,#23778,#23779,#23780,#23781,
#23782,#23783,#23784,#23785,#23786,#23787,#23788,#23789,#23790,#23791,#23792,
#23793,#23794,#23795,#23796,#23797,#23798,#23799,#23800,#23801,#23802,#23803,
#23804,#23805,#23806,#23807,#23808)),.UNSPECIFIED.,.F.,.F.,.F.,(4,4),(4,
1,1,1,1,1,1,1,1,1,1,1,1,1,1,1,1,1,1,1,1,1,1,1,1,1,1,1,1,1,1,1,1,1,4),(0.,
0.0661932083625904),(9.4992404446547,9.97150665008959,10.4437728555245,
10.9160390609594,11.3883052663942,11.8605714718291,12.332837677264,12.8051038826989,
13.2773700881338,13.7496362935687,14.2219024990035,14.6941687044384,15.1664349098733,
15.6387011153082,16.1109673207431,16.583233526178,17.0554997316128,17.5277659370477,
18.0000321424826,18.4722983479175,18.9445645533524,19.4168307587873,19.8890969642221,
20.361363169657,20.8336293750919,21.3058955805268,21.7781617859617,22.2504279913965,
22.7226941968314,23.1949604022663,23.6672266077012,24.1394928131361,24.611759018571,
25.0840252240059,25.5562914294407),.UNSPECIFIED.);
#493=B_SPLINE_SURFACE_WITH_KNOTS('',3,3,((#24122,#24123,#24124,#24125,#24126,
#24127,#24128,#24129,#24130,#24131,#24132,#24133,#24134,#24135,#24136,#24137,
#24138,#24139,#24140,#24141,#24142,#24143,#24144,#24145,#24146,#24147,#24148,
#24149,#24150,#24151,#24152),(#24153,#24154,#24155,#24156,#24157,#24158,
#24159,#24160,#24161,#24162,#24163,#24164,#24165,#24166,#24167,#24168,#24169,
#24170,#24171,#24172,#24173,#24174,#24175,#24176,#24177,#24178,#24179,#24180,
#24181,#24182,#24183),(#24184,#24185,#24186,#24187,#24188,#24189,#24190,
#24191,#24192,#24193,#24194,#24195,#24196,#24197,#24198,#24199,#24200,#24201,
#24202,#24203,#24204,#24205,#24206,#24207,#24208,#24209,#24210,#24211,#24212,
#24213,#24214),(#24215,#24216,#24217,#24218,#24219,#24220,#24221,#24222,
#24223,#24224,#24225,#24226,#24227,#24228,#24229,#24230,#24231,#24232,#24233,
#24234,#24235,#24236,#24237,#24238,#24239,#24240,#24241,#24242,#24243,#24244,
#24245)),.UNSPECIFIED.,.F.,.F.,.F.,(4,4),(4,1,1,1,1,1,1,1,1,1,1,1,1,1,1,
1,1,1,1,1,1,1,1,1,1,1,1,1,4),(0.,0.0661932083625904),(15.7493687799271,
16.2181316635384,16.6868945471497,17.155657430761,17.6244203143723,18.0931831979836,
18.5619460815949,19.0307089652062,19.4994718488175,19.9682347324288,20.4369976160401,
20.9057604996514,21.3745233832627,21.8432862668739,22.3120491504852,22.7808120340965,
23.2495749177078,23.7183378013191,24.1871006849304,24.6558635685417,25.124626452153,
25.5933893357643,26.0621522193756,26.5309151029869,26.9996779865982,27.4684408702095,
27.9372037538208,28.4059666374321,28.8747295210434),.UNSPECIFIED.);
#494=B_SPLINE_SURFACE_WITH_KNOTS('',3,3,((#24347,#24348,#24349,#24350,#24351,
#24352,#24353,#24354,#24355),(#24356,#24357,#24358,#24359,#24360,#24361,
#24362,#24363,#24364),(#24365,#24366,#24367,#24368,#24369,#24370,#24371,
#24372,#24373),(#24374,#24375,#24376,#24377,#24378,#24379,#24380,#24381,
#24382)),.UNSPECIFIED.,.F.,.F.,.F.,(4,4),(4,1,1,1,1,1,4),(0.,0.0661932083625904),
(12.6424782450754,12.9748140827407,13.6394857580714,13.9718215957368,14.6364932710675,
15.3011649463983,15.6335007840636),.UNSPECIFIED.);
#495=B_SPLINE_SURFACE_WITH_KNOTS('',3,3,((#24418,#24419,#24420,#24421,#24422),
(#24423,#24424,#24425,#24426,#24427),(#24428,#24429,#24430,#24431,#24432),
(#24433,#24434,#24435,#24436,#24437)),.UNSPECIFIED.,.F.,.F.,.F.,(4,4),(4,
1,4),(0.0383415492497091,0.0661932083625904),(11.6150328478183,11.9900267092154,
12.4900185244115),.UNSPECIFIED.);
#496=B_SPLINE_SURFACE_WITH_KNOTS('',3,3,((#24459,#24460,#24461,#24462,#24463),
(#24464,#24465,#24466,#24467,#24468),(#24469,#24470,#24471,#24472,#24473),
(#24474,#24475,#24476,#24477,#24478)),.UNSPECIFIED.,.F.,.F.,.F.,(4,4),(4,
1,4),(0.0327046027417864,0.0661932083625904),(8.2965947562157,8.82345511654988,
9.35031547688406),.UNSPECIFIED.);
#497=B_SPLINE_SURFACE_WITH_KNOTS('',3,3,((#25107,#25108,#25109,#25110,#25111,
#25112,#25113,#25114,#25115,#25116,#25117,#25118,#25119,#25120,#25121,#25122,
#25123,#25124,#25125,#25126,#25127,#25128,#25129,#25130,#25131,#25132,#25133,
#25134,#25135,#25136,#25137,#25138,#25139,#25140,#25141,#25142,#25143,#25144,
#25145,#25146,#25147,#25148,#25149,#25150),(#25151,#25152,#25153,#25154,
#25155,#25156,#25157,#25158,#25159,#25160,#25161,#25162,#25163,#25164,#25165,
#25166,#25167,#25168,#25169,#25170,#25171,#25172,#25173,#25174,#25175,#25176,
#25177,#25178,#25179,#25180,#25181,#25182,#25183,#25184,#25185,#25186,#25187,
#25188,#25189,#25190,#25191,#25192,#25193,#25194),(#25195,#25196,#25197,
#25198,#25199,#25200,#25201,#25202,#25203,#25204,#25205,#25206,#25207,#25208,
#25209,#25210,#25211,#25212,#25213,#25214,#25215,#25216,#25217,#25218,#25219,
#25220,#25221,#25222,#25223,#25224,#25225,#25226,#25227,#25228,#25229,#25230,
#25231,#25232,#25233,#25234,#25235,#25236,#25237,#25238),(#25239,#25240,
#25241,#25242,#25243,#25244,#25245,#25246,#25247,#25248,#25249,#25250,#25251,
#25252,#25253,#25254,#25255,#25256,#25257,#25258,#25259,#25260,#25261,#25262,
#25263,#25264,#25265,#25266,#25267,#25268,#25269,#25270,#25271,#25272,#25273,
#25274,#25275,#25276,#25277,#25278,#25279,#25280,#25281,#25282)),
 .UNSPECIFIED.,.F.,.F.,.F.,(4,4),(4,1,1,1,1,1,1,1,1,1,1,1,1,1,1,1,1,1,1,
1,1,1,1,1,1,1,1,1,1,1,1,1,1,1,1,1,1,1,1,1,1,4),(0.,0.0460148164544132),
(8.31058692273977,9.29723107803592,10.2838752333321,11.2705193886282,12.2571635439244,
13.2438076992205,14.2304518545166,15.2170960098128,16.2037401651089,17.1903843204051,
18.1770284757012,19.1636726309974,20.1503167862935,21.1369609415897,22.1236050968858,
23.110249252182,24.0968934074781,25.0835375627742,26.0701817180704,27.0568258733665,
28.0434700286627,29.0301141839588,30.016758339255,31.0034024945511,31.9900466498473,
32.9766908051434,33.9633349604396,34.9499791157357,35.9366232710318,36.923267426328,
37.9099115816241,38.8965557369203,39.8831998922164,40.8698440475126,41.8564882028087,
42.8431323581049,43.829776513401,44.8164206686971,45.8030648239933,46.7897089792894,
47.7763531345856,48.7629972898817),.UNSPECIFIED.);
#498=B_SPLINE_SURFACE_WITH_KNOTS('',3,3,((#25437,#25438,#25439,#25440,#25441,
#25442,#25443,#25444,#25445,#25446,#25447,#25448,#25449,#25450,#25451,#25452,
#25453,#25454,#25455,#25456,#25457,#25458,#25459,#25460,#25461,#25462,#25463,
#25464,#25465,#25466,#25467,#25468,#25469,#25470,#25471,#25472,#25473,#25474,
#25475,#25476,#25477,#25478,#25479,#25480),(#25481,#25482,#25483,#25484,
#25485,#25486,#25487,#25488,#25489,#25490,#25491,#25492,#25493,#25494,#25495,
#25496,#25497,#25498,#25499,#25500,#25501,#25502,#25503,#25504,#25505,#25506,
#25507,#25508,#25509,#25510,#25511,#25512,#25513,#25514,#25515,#25516,#25517,
#25518,#25519,#25520,#25521,#25522,#25523,#25524),(#25525,#25526,#25527,
#25528,#25529,#25530,#25531,#25532,#25533,#25534,#25535,#25536,#25537,#25538,
#25539,#25540,#25541,#25542,#25543,#25544,#25545,#25546,#25547,#25548,#25549,
#25550,#25551,#25552,#25553,#25554,#25555,#25556,#25557,#25558,#25559,#25560,
#25561,#25562,#25563,#25564,#25565,#25566,#25567,#25568),(#25569,#25570,
#25571,#25572,#25573,#25574,#25575,#25576,#25577,#25578,#25579,#25580,#25581,
#25582,#25583,#25584,#25585,#25586,#25587,#25588,#25589,#25590,#25591,#25592,
#25593,#25594,#25595,#25596,#25597,#25598,#25599,#25600,#25601,#25602,#25603,
#25604,#25605,#25606,#25607,#25608,#25609,#25610,#25611,#25612)),
 .UNSPECIFIED.,.F.,.F.,.F.,(4,4),(4,1,1,1,1,1,1,1,1,1,1,1,1,1,1,1,1,1,1,
1,1,1,1,1,1,1,1,1,1,1,1,1,1,1,1,1,1,1,1,1,1,4),(0.,0.0460148164544132),
(11.6154215191106,12.6020656744068,13.5887098297029,14.5753539849991,15.5619981402952,
16.5486422955914,17.5352864508875,18.5219306061837,19.5085747614798,20.4952189167759,
21.4818630720721,22.4685072273682,23.4551513826644,24.4417955379605,25.4284396932567,
26.4150838485528,27.401728003849,28.3883721591451,29.3750163144413,30.3616604697374,
31.3483046250335,32.3349487803297,33.3215929356258,34.308237090922,35.2948812462181,
36.2815254015143,37.2681695568104,38.2548137121066,39.2414578674027,40.2281020226988,
41.214746177995,42.2013903332911,43.1880344885873,44.1746786438834,45.1613227991796,
46.1479669544757,47.1346111097719,48.121255265068,49.1078994203642,50.0945435756603,
51.0811877309565,52.0678318862526),.UNSPECIFIED.);
#499=B_SPLINE_SURFACE_WITH_KNOTS('',3,3,((#26238,#26239,#26240,#26241,#26242,
#26243,#26244,#26245,#26246,#26247,#26248,#26249,#26250,#26251,#26252,#26253,
#26254,#26255,#26256,#26257,#26258,#26259,#26260,#26261,#26262,#26263,#26264,
#26265,#26266,#26267,#26268,#26269,#26270,#26271,#26272),(#26273,#26274,
#26275,#26276,#26277,#26278,#26279,#26280,#26281,#26282,#26283,#26284,#26285,
#26286,#26287,#26288,#26289,#26290,#26291,#26292,#26293,#26294,#26295,#26296,
#26297,#26298,#26299,#26300,#26301,#26302,#26303,#26304,#26305,#26306,#26307),
(#26308,#26309,#26310,#26311,#26312,#26313,#26314,#26315,#26316,#26317,
#26318,#26319,#26320,#26321,#26322,#26323,#26324,#26325,#26326,#26327,#26328,
#26329,#26330,#26331,#26332,#26333,#26334,#26335,#26336,#26337,#26338,#26339,
#26340,#26341,#26342),(#26343,#26344,#26345,#26346,#26347,#26348,#26349,
#26350,#26351,#26352,#26353,#26354,#26355,#26356,#26357,#26358,#26359,#26360,
#26361,#26362,#26363,#26364,#26365,#26366,#26367,#26368,#26369,#26370,#26371,
#26372,#26373,#26374,#26375,#26376,#26377)),.UNSPECIFIED.,.F.,.F.,.F.,(4,
4),(4,1,1,1,1,1,1,1,1,1,1,1,1,1,1,1,1,1,1,1,1,1,1,1,1,1,1,1,1,1,1,1,4),
(0.,0.0460148164544132),(8.31058692273978,9.29422540264245,10.2778638825451,
11.2615023624478,12.2451408423505,13.2287793222531,14.2124178021558,15.1960562820585,
16.1796947619611,17.1633332418638,18.1469717217665,19.1306102016691,20.1142486815718,
21.0978871614745,22.0815256413772,23.0651641212798,24.0488026011825,25.0324410810852,
26.0160795609878,26.9997180408905,27.9833565207932,28.9669950006958,29.9506334805985,
30.9342719605012,31.9179104404039,32.9015489203065,33.8851874002092,34.8688258801119,
35.8524643600145,36.8361028399172,37.8197413198199,38.8033797997225,39.7870182796252),
 .UNSPECIFIED.);
#500=B_SPLINE_SURFACE_WITH_KNOTS('',3,3,((#26523,#26524,#26525,#26526,#26527,
#26528,#26529,#26530,#26531,#26532,#26533,#26534,#26535,#26536,#26537,#26538,
#26539,#26540,#26541,#26542,#26543,#26544,#26545,#26546,#26547,#26548,#26549,
#26550,#26551,#26552,#26553,#26554,#26555,#26556,#26557),(#26558,#26559,
#26560,#26561,#26562,#26563,#26564,#26565,#26566,#26567,#26568,#26569,#26570,
#26571,#26572,#26573,#26574,#26575,#26576,#26577,#26578,#26579,#26580,#26581,
#26582,#26583,#26584,#26585,#26586,#26587,#26588,#26589,#26590,#26591,#26592),
(#26593,#26594,#26595,#26596,#26597,#26598,#26599,#26600,#26601,#26602,
#26603,#26604,#26605,#26606,#26607,#26608,#26609,#26610,#26611,#26612,#26613,
#26614,#26615,#26616,#26617,#26618,#26619,#26620,#26621,#26622,#26623,#26624,
#26625,#26626,#26627),(#26628,#26629,#26630,#26631,#26632,#26633,#26634,
#26635,#26636,#26637,#26638,#26639,#26640,#26641,#26642,#26643,#26644,#26645,
#26646,#26647,#26648,#26649,#26650,#26651,#26652,#26653,#26654,#26655,#26656,
#26657,#26658,#26659,#26660,#26661,#26662)),.UNSPECIFIED.,.F.,.F.,.F.,(4,
4),(4,1,1,1,1,1,1,1,1,1,1,1,1,1,1,1,1,1,1,1,1,1,1,1,1,1,1,1,1,1,1,1,4),
(0.,0.0460148164544132),(11.6154215191106,12.5990599990133,13.582698478916,
14.5663369588187,15.5499754387213,16.533613918624,17.5172523985267,18.5008908784293,
19.484529358332,20.4681678382347,21.4518063181373,22.43544479804,23.4190832779427,
24.4027217578453,25.386360237748,26.3699987176507,27.3536371975534,28.337275677456,
29.3209141573587,30.3045526372614,31.288191117164,32.2718295970667,33.2554680769694,
34.239106556872,35.2227450367747,36.2063835166774,37.19002199658,38.1736604764827,
39.1572989563854,40.1409374362881,41.1245759161907,42.1082143960934,43.0918528759961),
 .UNSPECIFIED.);
#501=B_SPLINE_SURFACE_WITH_KNOTS('',3,3,((#26897,#26898,#26899,#26900,#26901,
#26902,#26903,#26904,#26905,#26906,#26907,#26908,#26909,#26910,#26911,#26912,
#26913,#26914,#26915,#26916,#26917,#26918,#26919,#26920,#26921,#26922,#26923,
#26924,#26925,#26926),(#26927,#26928,#26929,#26930,#26931,#26932,#26933,
#26934,#26935,#26936,#26937,#26938,#26939,#26940,#26941,#26942,#26943,#26944,
#26945,#26946,#26947,#26948,#26949,#26950,#26951,#26952,#26953,#26954,#26955,
#26956),(#26957,#26958,#26959,#26960,#26961,#26962,#26963,#26964,#26965,
#26966,#26967,#26968,#26969,#26970,#26971,#26972,#26973,#26974,#26975,#26976,
#26977,#26978,#26979,#26980,#26981,#26982,#26983,#26984,#26985,#26986),
(#26987,#26988,#26989,#26990,#26991,#26992,#26993,#26994,#26995,#26996,
#26997,#26998,#26999,#27000,#27001,#27002,#27003,#27004,#27005,#27006,#27007,
#27008,#27009,#27010,#27011,#27012,#27013,#27014,#27015,#27016)),
 .UNSPECIFIED.,.F.,.T.,.F.,(4,4),(4,1,1,1,1,1,1,1,2,2,2,2,1,1,1,1,1,1,1,
2,2,4),(0.,1.),(0.,0.0483649312414982,0.0967298624829964,0.145094793724495,
0.193459724965993,0.241824656207491,0.290189587448989,0.326463285880113,
0.386919449931986,0.464302426118159,0.541687686804892,0.619072947491625,
0.677110750756395,0.735148554021165,0.793186357285935,0.851224160550705,
0.909261963815475,0.967299767080245,0.99631866871263,1.08337537360978,1.16076063429652,
1.23814589498325),.UNSPECIFIED.);
#502=B_SPLINE_SURFACE_WITH_KNOTS('',3,3,((#27146,#27147,#27148,#27149,#27150,
#27151,#27152,#27153,#27154,#27155,#27156,#27157,#27158,#27159,#27160,#27161,
#27162,#27163,#27164,#27165,#27166,#27167,#27168,#27169,#27170,#27171),
(#27172,#27173,#27174,#27175,#27176,#27177,#27178,#27179,#27180,#27181,
#27182,#27183,#27184,#27185,#27186,#27187,#27188,#27189,#27190,#27191,#27192,
#27193,#27194,#27195,#27196,#27197),(#27198,#27199,#27200,#27201,#27202,
#27203,#27204,#27205,#27206,#27207,#27208,#27209,#27210,#27211,#27212,#27213,
#27214,#27215,#27216,#27217,#27218,#27219,#27220,#27221,#27222,#27223),
(#27224,#27225,#27226,#27227,#27228,#27229,#27230,#27231,#27232,#27233,
#27234,#27235,#27236,#27237,#27238,#27239,#27240,#27241,#27242,#27243,#27244,
#27245,#27246,#27247,#27248,#27249)),.UNSPECIFIED.,.F.,.T.,.F.,(4,4),(4,
2,2,2,2,2,1,1,1,1,1,1,1,2,2,1,4),(0.,1.),(0.358934429201528,0.49197868985962,
0.564785636730508,0.596617469546802,0.699442998635822,0.77716819339067,
0.842568141080894,0.907968088771118,0.973368036461342,1.03876798415157,
1.07146795799668,1.10416793184179,1.16956787953201,1.30036777491246,1.39600843428647,
1.50005496459849,1.6041014949105),.UNSPECIFIED.);
#503=B_SPLINE_SURFACE_WITH_KNOTS('',3,3,((#29345,#29346,#29347,#29348,#29349,
#29350,#29351,#29352,#29353,#29354,#29355,#29356,#29357,#29358,#29359,#29360,
#29361,#29362,#29363,#29364,#29365,#29366,#29367,#29368,#29369,#29370,#29371,
#29372,#29373,#29374,#29375,#29376,#29377,#29378,#29379,#29380,#29381,#29382,
#29383,#29384,#29385,#29386,#29387,#29388,#29389,#29390,#29391,#29392,#29393,
#29394,#29395,#29396,#29397,#29398,#29399,#29400,#29401,#29402,#29403,#29404,
#29405,#29406,#29407,#29408,#29409,#29410,#29411,#29412,#29413,#29414,#29415,
#29416,#29417,#29418,#29419,#29420,#29421,#29422,#29423,#29424,#29425,#29426,
#29427,#29428,#29429,#29430,#29431,#29432,#29433,#29434,#29435,#29436,#29437,
#29438,#29439,#29440,#29441,#29442,#29443,#29444,#29445,#29446,#29447,#29448,
#29449,#29450,#29451,#29452,#29453,#29454,#29455,#29456,#29457,#29458,#29459,
#29460,#29461,#29462,#29463,#29464,#29465,#29466,#29467,#29468,#29469,#29470,
#29471,#29472,#29473,#29474,#29475,#29476,#29477,#29478,#29479,#29480,#29481,
#29482,#29483,#29484,#29485,#29486,#29487,#29488,#29489,#29490,#29491,#29492,
#29493,#29494,#29495,#29496),(#29497,#29498,#29499,#29500,#29501,#29502,
#29503,#29504,#29505,#29506,#29507,#29508,#29509,#29510,#29511,#29512,#29513,
#29514,#29515,#29516,#29517,#29518,#29519,#29520,#29521,#29522,#29523,#29524,
#29525,#29526,#29527,#29528,#29529,#29530,#29531,#29532,#29533,#29534,#29535,
#29536,#29537,#29538,#29539,#29540,#29541,#29542,#29543,#29544,#29545,#29546,
#29547,#29548,#29549,#29550,#29551,#29552,#29553,#29554,#29555,#29556,#29557,
#29558,#29559,#29560,#29561,#29562,#29563,#29564,#29565,#29566,#29567,#29568,
#29569,#29570,#29571,#29572,#29573,#29574,#29575,#29576,#29577,#29578,#29579,
#29580,#29581,#29582,#29583,#29584,#29585,#29586,#29587,#29588,#29589,#29590,
#29591,#29592,#29593,#29594,#29595,#29596,#29597,#29598,#29599,#29600,#29601,
#29602,#29603,#29604,#29605,#29606,#29607,#29608,#29609,#29610,#29611,#29612,
#29613,#29614,#29615,#29616,#29617,#29618,#29619,#29620,#29621,#29622,#29623,
#29624,#29625,#29626,#29627,#29628,#29629,#29630,#29631,#29632,#29633,#29634,
#29635,#29636,#29637,#29638,#29639,#29640,#29641,#29642,#29643,#29644,#29645,
#29646,#29647,#29648),(#29649,#29650,#29651,#29652,#29653,#29654,#29655,
#29656,#29657,#29658,#29659,#29660,#29661,#29662,#29663,#29664,#29665,#29666,
#29667,#29668,#29669,#29670,#29671,#29672,#29673,#29674,#29675,#29676,#29677,
#29678,#29679,#29680,#29681,#29682,#29683,#29684,#29685,#29686,#29687,#29688,
#29689,#29690,#29691,#29692,#29693,#29694,#29695,#29696,#29697,#29698,#29699,
#29700,#29701,#29702,#29703,#29704,#29705,#29706,#29707,#29708,#29709,#29710,
#29711,#29712,#29713,#29714,#29715,#29716,#29717,#29718,#29719,#29720,#29721,
#29722,#29723,#29724,#29725,#29726,#29727,#29728,#29729,#29730,#29731,#29732,
#29733,#29734,#29735,#29736,#29737,#29738,#29739,#29740,#29741,#29742,#29743,
#29744,#29745,#29746,#29747,#29748,#29749,#29750,#29751,#29752,#29753,#29754,
#29755,#29756,#29757,#29758,#29759,#29760,#29761,#29762,#29763,#29764,#29765,
#29766,#29767,#29768,#29769,#29770,#29771,#29772,#29773,#29774,#29775,#29776,
#29777,#29778,#29779,#29780,#29781,#29782,#29783,#29784,#29785,#29786,#29787,
#29788,#29789,#29790,#29791,#29792,#29793,#29794,#29795,#29796,#29797,#29798,
#29799,#29800),(#29801,#29802,#29803,#29804,#29805,#29806,#29807,#29808,
#29809,#29810,#29811,#29812,#29813,#29814,#29815,#29816,#29817,#29818,#29819,
#29820,#29821,#29822,#29823,#29824,#29825,#29826,#29827,#29828,#29829,#29830,
#29831,#29832,#29833,#29834,#29835,#29836,#29837,#29838,#29839,#29840,#29841,
#29842,#29843,#29844,#29845,#29846,#29847,#29848,#29849,#29850,#29851,#29852,
#29853,#29854,#29855,#29856,#29857,#29858,#29859,#29860,#29861,#29862,#29863,
#29864,#29865,#29866,#29867,#29868,#29869,#29870,#29871,#29872,#29873,#29874,
#29875,#29876,#29877,#29878,#29879,#29880,#29881,#29882,#29883,#29884,#29885,
#29886,#29887,#29888,#29889,#29890,#29891,#29892,#29893,#29894,#29895,#29896,
#29897,#29898,#29899,#29900,#29901,#29902,#29903,#29904,#29905,#29906,#29907,
#29908,#29909,#29910,#29911,#29912,#29913,#29914,#29915,#29916,#29917,#29918,
#29919,#29920,#29921,#29922,#29923,#29924,#29925,#29926,#29927,#29928,#29929,
#29930,#29931,#29932,#29933,#29934,#29935,#29936,#29937,#29938,#29939,#29940,
#29941,#29942,#29943,#29944,#29945,#29946,#29947,#29948,#29949,#29950,#29951,
#29952)),.UNSPECIFIED.,.F.,.F.,.F.,(4,4),(4,1,1,1,1,1,1,1,1,1,1,1,1,1,1,
1,1,1,1,1,1,1,1,1,1,1,1,1,1,1,1,1,1,1,1,1,1,1,1,1,1,1,1,1,1,1,1,1,1,1,1,
1,1,1,1,1,1,1,1,1,1,1,1,1,1,1,1,1,1,1,1,1,1,1,1,1,1,1,1,1,1,1,1,1,1,1,1,
1,1,1,1,1,1,1,1,1,1,1,1,1,1,1,1,1,1,1,1,1,1,1,1,1,1,1,1,1,1,1,1,1,1,1,1,
1,1,1,1,1,1,1,1,1,1,1,1,1,1,1,1,1,1,1,1,1,1,1,1,1,1,4),(0.,0.0329955678841871),
(8.30276167405409,9.29807539437161,10.2933891146891,11.2887028350066,12.2840165553242,
13.2793302756417,14.2746439959592,15.2699577162767,16.2652714365942,17.2605851569118,
18.2558988772293,19.2512125975468,20.2465263178643,21.2418400381818,22.2371537584993,
23.2324674788169,24.2277811991344,25.2230949194519,26.2184086397694,27.2137223600869,
28.2090360804045,29.204349800722,30.1996635210395,31.194977241357,32.1902909616745,
33.185604681992,34.1809184023096,35.1762321226271,36.1715458429446,37.1668595632621,
38.1621732835796,39.1574870038972,40.1528007242147,41.1481144445322,42.1434281648497,
43.1387418851672,44.1340556054847,45.1293693258023,46.1246830461198,47.1199967664373,
48.1153104867548,49.1106242070723,50.1059379273898,51.1012516477074,52.0965653680249,
53.0918790883424,54.0871928086599,55.0825065289774,56.077820249295,57.0731339696125,
58.06844768993,59.0637614102475,60.059075130565,61.0543888508825,62.0497025712001,
63.0450162915176,64.0403300118351,65.0356437321526,66.0309574524701,67.0262711727877,
68.0215848931052,69.0168986134227,70.0122123337402,71.0075260540577,72.0028397743752,
72.9981534946928,73.9934672150103,74.9887809353278,75.9840946556453,76.9794083759628,
77.9747220962804,78.9700358165979,79.9653495369154,80.9606632572329,81.9559769775504,
82.9512906978679,83.9466044181855,84.941918138503,85.9372318588205,86.932545579138,
87.9278592994555,88.9231730197731,89.9184867400906,90.9138004604081,91.9091141807256,
92.9044279010431,93.8997416213606,94.8950553416782,95.8903690619957,96.8856827823132,
97.8809965026307,98.8763102229482,99.8716239432658,100.866937663583,101.862251383901,
102.857565104218,103.852878824536,104.848192544853,105.843506265171,106.838819985488,
107.834133705806,108.829447426123,109.824761146441,110.820074866758,111.815388587076,
112.810702307393,113.806016027711,114.801329748029,115.796643468346,116.791957188664,
117.787270908981,118.782584629299,119.777898349616,120.773212069934,121.768525790251,
122.763839510569,123.759153230886,124.754466951204,125.749780671521,126.745094391839,
127.740408112156,128.735721832474,129.731035552791,130.726349273109,131.721662993426,
132.716976713744,133.712290434061,134.707604154379,135.702917874696,136.698231595014,
137.693545315331,138.688859035649,139.684172755966,140.679486476284,141.674800196602,
142.670113916919,143.665427637237,144.660741357554,145.656055077872,146.651368798189,
147.646682518507,148.641996238824,149.637309959142,150.632623679459,151.627937399777,
152.623251120094,153.618564840412,154.613878560729,155.609192281047,156.604506001364),
 .UNSPECIFIED.);
#504=B_SPLINE_SURFACE_WITH_KNOTS('',3,3,((#30148,#30149,#30150,#30151,#30152,
#30153,#30154,#30155,#30156,#30157,#30158,#30159,#30160,#30161,#30162,#30163,
#30164,#30165,#30166,#30167,#30168,#30169,#30170,#30171,#30172,#30173,#30174,
#30175,#30176,#30177,#30178,#30179,#30180,#30181,#30182,#30183,#30184,#30185,
#30186,#30187,#30188,#30189,#30190,#30191,#30192,#30193,#30194,#30195,#30196,
#30197,#30198,#30199,#30200,#30201,#30202,#30203,#30204,#30205,#30206,#30207,
#30208,#30209,#30210,#30211,#30212,#30213,#30214,#30215,#30216,#30217,#30218,
#30219,#30220,#30221,#30222,#30223,#30224,#30225,#30226,#30227,#30228,#30229,
#30230,#30231,#30232,#30233,#30234,#30235,#30236,#30237,#30238,#30239,#30240,
#30241,#30242,#30243,#30244,#30245,#30246,#30247,#30248,#30249,#30250,#30251,
#30252,#30253,#30254,#30255,#30256,#30257,#30258,#30259,#30260,#30261,#30262,
#30263,#30264,#30265,#30266,#30267,#30268,#30269,#30270,#30271,#30272,#30273,
#30274,#30275,#30276,#30277,#30278,#30279,#30280,#30281,#30282,#30283,#30284,
#30285,#30286,#30287,#30288,#30289,#30290,#30291,#30292,#30293,#30294,#30295,
#30296,#30297,#30298,#30299),(#30300,#30301,#30302,#30303,#30304,#30305,
#30306,#30307,#30308,#30309,#30310,#30311,#30312,#30313,#30314,#30315,#30316,
#30317,#30318,#30319,#30320,#30321,#30322,#30323,#30324,#30325,#30326,#30327,
#30328,#30329,#30330,#30331,#30332,#30333,#30334,#30335,#30336,#30337,#30338,
#30339,#30340,#30341,#30342,#30343,#30344,#30345,#30346,#30347,#30348,#30349,
#30350,#30351,#30352,#30353,#30354,#30355,#30356,#30357,#30358,#30359,#30360,
#30361,#30362,#30363,#30364,#30365,#30366,#30367,#30368,#30369,#30370,#30371,
#30372,#30373,#30374,#30375,#30376,#30377,#30378,#30379,#30380,#30381,#30382,
#30383,#30384,#30385,#30386,#30387,#30388,#30389,#30390,#30391,#30392,#30393,
#30394,#30395,#30396,#30397,#30398,#30399,#30400,#30401,#30402,#30403,#30404,
#30405,#30406,#30407,#30408,#30409,#30410,#30411,#30412,#30413,#30414,#30415,
#30416,#30417,#30418,#30419,#30420,#30421,#30422,#30423,#30424,#30425,#30426,
#30427,#30428,#30429,#30430,#30431,#30432,#30433,#30434,#30435,#30436,#30437,
#30438,#30439,#30440,#30441,#30442,#30443,#30444,#30445,#30446,#30447,#30448,
#30449,#30450,#30451),(#30452,#30453,#30454,#30455,#30456,#30457,#30458,
#30459,#30460,#30461,#30462,#30463,#30464,#30465,#30466,#30467,#30468,#30469,
#30470,#30471,#30472,#30473,#30474,#30475,#30476,#30477,#30478,#30479,#30480,
#30481,#30482,#30483,#30484,#30485,#30486,#30487,#30488,#30489,#30490,#30491,
#30492,#30493,#30494,#30495,#30496,#30497,#30498,#30499,#30500,#30501,#30502,
#30503,#30504,#30505,#30506,#30507,#30508,#30509,#30510,#30511,#30512,#30513,
#30514,#30515,#30516,#30517,#30518,#30519,#30520,#30521,#30522,#30523,#30524,
#30525,#30526,#30527,#30528,#30529,#30530,#30531,#30532,#30533,#30534,#30535,
#30536,#30537,#30538,#30539,#30540,#30541,#30542,#30543,#30544,#30545,#30546,
#30547,#30548,#30549,#30550,#30551,#30552,#30553,#30554,#30555,#30556,#30557,
#30558,#30559,#30560,#30561,#30562,#30563,#30564,#30565,#30566,#30567,#30568,
#30569,#30570,#30571,#30572,#30573,#30574,#30575,#30576,#30577,#30578,#30579,
#30580,#30581,#30582,#30583,#30584,#30585,#30586,#30587,#30588,#30589,#30590,
#30591,#30592,#30593,#30594,#30595,#30596,#30597,#30598,#30599,#30600,#30601,
#30602,#30603),(#30604,#30605,#30606,#30607,#30608,#30609,#30610,#30611,
#30612,#30613,#30614,#30615,#30616,#30617,#30618,#30619,#30620,#30621,#30622,
#30623,#30624,#30625,#30626,#30627,#30628,#30629,#30630,#30631,#30632,#30633,
#30634,#30635,#30636,#30637,#30638,#30639,#30640,#30641,#30642,#30643,#30644,
#30645,#30646,#30647,#30648,#30649,#30650,#30651,#30652,#30653,#30654,#30655,
#30656,#30657,#30658,#30659,#30660,#30661,#30662,#30663,#30664,#30665,#30666,
#30667,#30668,#30669,#30670,#30671,#30672,#30673,#30674,#30675,#30676,#30677,
#30678,#30679,#30680,#30681,#30682,#30683,#30684,#30685,#30686,#30687,#30688,
#30689,#30690,#30691,#30692,#30693,#30694,#30695,#30696,#30697,#30698,#30699,
#30700,#30701,#30702,#30703,#30704,#30705,#30706,#30707,#30708,#30709,#30710,
#30711,#30712,#30713,#30714,#30715,#30716,#30717,#30718,#30719,#30720,#30721,
#30722,#30723,#30724,#30725,#30726,#30727,#30728,#30729,#30730,#30731,#30732,
#30733,#30734,#30735,#30736,#30737,#30738,#30739,#30740,#30741,#30742,#30743,
#30744,#30745,#30746,#30747,#30748,#30749,#30750,#30751,#30752,#30753,#30754,
#30755)),.UNSPECIFIED.,.F.,.F.,.F.,(4,4),(4,1,1,1,1,1,1,1,1,1,1,1,1,1,1,
1,1,1,1,1,1,1,1,1,1,1,1,1,1,1,1,1,1,1,1,1,1,1,1,1,1,1,1,1,1,1,1,1,1,1,1,
1,1,1,1,1,1,1,1,1,1,1,1,1,1,1,1,1,1,1,1,1,1,1,1,1,1,1,1,1,1,1,1,1,1,1,1,
1,1,1,1,1,1,1,1,1,1,1,1,1,1,1,1,1,1,1,1,1,1,1,1,1,1,1,1,1,1,1,1,1,1,1,1,
1,1,1,1,1,1,1,1,1,1,1,1,1,1,1,1,1,1,1,1,1,1,1,1,1,1,4),(0.,0.0329955678841871),
(11.6152142277548,12.6105279480723,13.6058416683898,14.6011553887073,15.5964691090248,
16.5917828293423,17.5870965496599,18.5824102699774,19.5777239902949,20.5730377106124,
21.5683514309299,22.5636651512475,23.558978871565,24.5542925918825,25.5496063122,
26.5449200325175,27.540233752835,28.5355474731526,29.5308611934701,30.5261749137876,
31.5214886341051,32.5168023544226,33.5121160747401,34.5074297950577,35.5027435153752,
36.4980572356927,37.4933709560102,38.4886846763277,39.4839983966453,40.4793121169628,
41.4746258372803,42.4699395575978,43.4652532779153,44.4605669982328,45.4558807185504,
46.4511944388679,47.4465081591854,48.4418218795029,49.4371355998204,50.432449320138,
51.4277630404555,52.423076760773,53.4183904810905,54.413704201408,55.4090179217255,
56.4043316420431,57.3996453623606,58.3949590826781,59.3902728029956,60.3855865233131,
61.3809002436307,62.3762139639482,63.3715276842657,64.3668414045832,65.3621551249007,
66.3574688452182,67.3527825655358,68.3480962858533,69.3434100061708,70.3387237264883,
71.3340374468058,72.3293511671233,73.3246648874409,74.3199786077584,75.3152923280759,
76.3106060483934,77.3059197687109,78.3012334890285,79.296547209346,80.2918609296635,
81.287174649981,82.2824883702986,83.2778020906161,84.2731158109336,85.2684295312511,
86.2637432515686,87.2590569718861,88.2543706922037,89.2496844125212,90.2449981328387,
91.2403118531562,92.2356255734737,93.2309392937912,94.2262530141087,95.2215667344263,
96.2168804547438,97.2121941750613,98.2075078953788,99.2028216156963,100.198135336014,
101.193449056331,102.188762776649,103.184076496966,104.179390217284,105.174703937601,
106.170017657919,107.165331378236,108.160645098554,109.155958818872,110.151272539189,
111.146586259507,112.141899979824,113.137213700142,114.132527420459,115.127841140777,
116.123154861094,117.118468581412,118.113782301729,119.109096022047,120.104409742364,
121.099723462682,122.095037182999,123.090350903317,124.085664623634,125.080978343952,
126.076292064269,127.071605784587,128.066919504904,129.062233225222,130.057546945539,
131.052860665857,132.048174386174,133.043488106492,134.038801826809,135.034115547127,
136.029429267445,137.024742987762,138.02005670808,139.015370428397,140.010684148715,
141.005997869032,142.00131158935,142.996625309667,143.991939029985,144.987252750302,
145.98256647062,146.977880190937,147.973193911255,148.968507631572,149.96382135189,
150.959135072207,151.954448792525,152.949762512842,153.94507623316,154.940389953477,
155.935703673795,156.931017394112,157.92633111443,158.921644834747,159.916958555065),
 .UNSPECIFIED.);
#505=B_SPLINE_SURFACE_WITH_KNOTS('',3,3,((#31614,#31615,#31616,#31617,#31618,
#31619,#31620,#31621,#31622,#31623,#31624,#31625,#31626,#31627,#31628,#31629,
#31630,#31631,#31632,#31633,#31634,#31635,#31636,#31637,#31638,#31639,#31640,
#31641,#31642,#31643,#31644,#31645,#31646,#31647,#31648,#31649,#31650,#31651,
#31652,#31653,#31654,#31655,#31656,#31657,#31658,#31659,#31660,#31661,#31662,
#31663,#31664,#31665,#31666,#31667),(#31668,#31669,#31670,#31671,#31672,
#31673,#31674,#31675,#31676,#31677,#31678,#31679,#31680,#31681,#31682,#31683,
#31684,#31685,#31686,#31687,#31688,#31689,#31690,#31691,#31692,#31693,#31694,
#31695,#31696,#31697,#31698,#31699,#31700,#31701,#31702,#31703,#31704,#31705,
#31706,#31707,#31708,#31709,#31710,#31711,#31712,#31713,#31714,#31715,#31716,
#31717,#31718,#31719,#31720,#31721),(#31722,#31723,#31724,#31725,#31726,
#31727,#31728,#31729,#31730,#31731,#31732,#31733,#31734,#31735,#31736,#31737,
#31738,#31739,#31740,#31741,#31742,#31743,#31744,#31745,#31746,#31747,#31748,
#31749,#31750,#31751,#31752,#31753,#31754,#31755,#31756,#31757,#31758,#31759,
#31760,#31761,#31762,#31763,#31764,#31765,#31766,#31767,#31768,#31769,#31770,
#31771,#31772,#31773,#31774,#31775),(#31776,#31777,#31778,#31779,#31780,
#31781,#31782,#31783,#31784,#31785,#31786,#31787,#31788,#31789,#31790,#31791,
#31792,#31793,#31794,#31795,#31796,#31797,#31798,#31799,#31800,#31801,#31802,
#31803,#31804,#31805,#31806,#31807,#31808,#31809,#31810,#31811,#31812,#31813,
#31814,#31815,#31816,#31817,#31818,#31819,#31820,#31821,#31822,#31823,#31824,
#31825,#31826,#31827,#31828,#31829),(#31830,#31831,#31832,#31833,#31834,
#31835,#31836,#31837,#31838,#31839,#31840,#31841,#31842,#31843,#31844,#31845,
#31846,#31847,#31848,#31849,#31850,#31851,#31852,#31853,#31854,#31855,#31856,
#31857,#31858,#31859,#31860,#31861,#31862,#31863,#31864,#31865,#31866,#31867,
#31868,#31869,#31870,#31871,#31872,#31873,#31874,#31875,#31876,#31877,#31878,
#31879,#31880,#31881,#31882,#31883),(#31884,#31885,#31886,#31887,#31888,
#31889,#31890,#31891,#31892,#31893,#31894,#31895,#31896,#31897,#31898,#31899,
#31900,#31901,#31902,#31903,#31904,#31905,#31906,#31907,#31908,#31909,#31910,
#31911,#31912,#31913,#31914,#31915,#31916,#31917,#31918,#31919,#31920,#31921,
#31922,#31923,#31924,#31925,#31926,#31927,#31928,#31929,#31930,#31931,#31932,
#31933,#31934,#31935,#31936,#31937),(#31938,#31939,#31940,#31941,#31942,
#31943,#31944,#31945,#31946,#31947,#31948,#31949,#31950,#31951,#31952,#31953,
#31954,#31955,#31956,#31957,#31958,#31959,#31960,#31961,#31962,#31963,#31964,
#31965,#31966,#31967,#31968,#31969,#31970,#31971,#31972,#31973,#31974,#31975,
#31976,#31977,#31978,#31979,#31980,#31981,#31982,#31983,#31984,#31985,#31986,
#31987,#31988,#31989,#31990,#31991),(#31992,#31993,#31994,#31995,#31996,
#31997,#31998,#31999,#32000,#32001,#32002,#32003,#32004,#32005,#32006,#32007,
#32008,#32009,#32010,#32011,#32012,#32013,#32014,#32015,#32016,#32017,#32018,
#32019,#32020,#32021,#32022,#32023,#32024,#32025,#32026,#32027,#32028,#32029,
#32030,#32031,#32032,#32033,#32034,#32035,#32036,#32037,#32038,#32039,#32040,
#32041,#32042,#32043,#32044,#32045),(#32046,#32047,#32048,#32049,#32050,
#32051,#32052,#32053,#32054,#32055,#32056,#32057,#32058,#32059,#32060,#32061,
#32062,#32063,#32064,#32065,#32066,#32067,#32068,#32069,#32070,#32071,#32072,
#32073,#32074,#32075,#32076,#32077,#32078,#32079,#32080,#32081,#32082,#32083,
#32084,#32085,#32086,#32087,#32088,#32089,#32090,#32091,#32092,#32093,#32094,
#32095,#32096,#32097,#32098,#32099),(#32100,#32101,#32102,#32103,#32104,
#32105,#32106,#32107,#32108,#32109,#32110,#32111,#32112,#32113,#32114,#32115,
#32116,#32117,#32118,#32119,#32120,#32121,#32122,#32123,#32124,#32125,#32126,
#32127,#32128,#32129,#32130,#32131,#32132,#32133,#32134,#32135,#32136,#32137,
#32138,#32139,#32140,#32141,#32142,#32143,#32144,#32145,#32146,#32147,#32148,
#32149,#32150,#32151,#32152,#32153),(#32154,#32155,#32156,#32157,#32158,
#32159,#32160,#32161,#32162,#32163,#32164,#32165,#32166,#32167,#32168,#32169,
#32170,#32171,#32172,#32173,#32174,#32175,#32176,#32177,#32178,#32179,#32180,
#32181,#32182,#32183,#32184,#32185,#32186,#32187,#32188,#32189,#32190,#32191,
#32192,#32193,#32194,#32195,#32196,#32197,#32198,#32199,#32200,#32201,#32202,
#32203,#32204,#32205,#32206,#32207)),.UNSPECIFIED.,.T.,.F.,.F.,(4,1,1,1,
1,1,1,1,4),(4,1,1,1,1,1,1,1,1,1,1,1,1,1,1,1,1,1,1,1,1,1,1,1,1,1,1,1,1,1,
1,1,1,1,1,1,1,1,1,1,1,1,1,1,1,1,1,1,1,1,1,4),(-3.14159265358979,-2.46839422782055,
-2.24399475256414,-1.34639685153848,-0.448798950512828,0.448798950512828,
1.34639685153848,2.24399475256414,3.14159265358979),(0.,0.0178571428571429,
0.0357142857142857,0.0535714285714286,0.0714285714285714,0.0892857142857143,
0.107142857142857,0.125,0.133928571428571,0.138392857142857,0.142857142857143,
0.166666666666667,0.19047619047619,0.214285714285714,0.232142857142857,
0.25,0.267857142857143,0.285714285714286,0.303571428571429,0.321428571428571,
0.339285714285714,0.357142857142857,0.375,0.392857142857143,0.428571428571429,
0.464285714285714,0.5,0.535714285714286,0.553571428571429,0.571428571428571,
0.589285714285714,0.607142857142857,0.625,0.642857142857143,0.660714285714286,
0.678571428571428,0.696428571428571,0.714285714285714,0.738095238095238,
0.761904761904762,0.785714285714286,0.809523809523809,0.833333333333333,
0.857142857142857,0.875,0.892857142857143,0.910714285714286,0.928571428571429,
0.946428571428571,0.964285714285714,0.982142857142857,1.),.UNSPECIFIED.);
#506=B_SPLINE_SURFACE_WITH_KNOTS('',3,3,((#33981,#33982,#33983,#33984,#33985,
#33986,#33987,#33988,#33989,#33990,#33991,#33992,#33993,#33994,#33995,#33996,
#33997,#33998,#33999,#34000,#34001,#34002,#34003,#34004,#34005,#34006,#34007,
#34008,#34009,#34010,#34011,#34012,#34013,#34014,#34015,#34016,#34017,#34018,
#34019,#34020,#34021,#34022,#34023,#34024,#34025,#34026,#34027,#34028,#34029,
#34030,#34031,#34032,#34033,#34034,#34035,#34036,#34037,#34038,#34039,#34040,
#34041,#34042,#34043,#34044,#34045,#34046,#34047,#34048,#34049,#34050,#34051,
#34052,#34053,#34054,#34055,#34056,#34057,#34058,#34059,#34060,#34061,#34062,
#34063,#34064,#34065,#34066,#34067,#34068,#34069,#34070,#34071,#34072,#34073,
#34074,#34075,#34076,#34077,#34078,#34079,#34080,#34081,#34082,#34083,#34084,
#34085,#34086,#34087,#34088,#34089,#34090,#34091,#34092,#34093,#34094,#34095,
#34096,#34097,#34098,#34099,#34100,#34101,#34102,#34103,#34104,#34105,#34106,
#34107,#34108,#34109,#34110,#34111,#34112,#34113,#34114,#34115,#34116,#34117,
#34118,#34119,#34120,#34121,#34122,#34123,#34124),(#34125,#34126,#34127,
#34128,#34129,#34130,#34131,#34132,#34133,#34134,#34135,#34136,#34137,#34138,
#34139,#34140,#34141,#34142,#34143,#34144,#34145,#34146,#34147,#34148,#34149,
#34150,#34151,#34152,#34153,#34154,#34155,#34156,#34157,#34158,#34159,#34160,
#34161,#34162,#34163,#34164,#34165,#34166,#34167,#34168,#34169,#34170,#34171,
#34172,#34173,#34174,#34175,#34176,#34177,#34178,#34179,#34180,#34181,#34182,
#34183,#34184,#34185,#34186,#34187,#34188,#34189,#34190,#34191,#34192,#34193,
#34194,#34195,#34196,#34197,#34198,#34199,#34200,#34201,#34202,#34203,#34204,
#34205,#34206,#34207,#34208,#34209,#34210,#34211,#34212,#34213,#34214,#34215,
#34216,#34217,#34218,#34219,#34220,#34221,#34222,#34223,#34224,#34225,#34226,
#34227,#34228,#34229,#34230,#34231,#34232,#34233,#34234,#34235,#34236,#34237,
#34238,#34239,#34240,#34241,#34242,#34243,#34244,#34245,#34246,#34247,#34248,
#34249,#34250,#34251,#34252,#34253,#34254,#34255,#34256,#34257,#34258,#34259,
#34260,#34261,#34262,#34263,#34264,#34265,#34266,#34267,#34268),(#34269,
#34270,#34271,#34272,#34273,#34274,#34275,#34276,#34277,#34278,#34279,#34280,
#34281,#34282,#34283,#34284,#34285,#34286,#34287,#34288,#34289,#34290,#34291,
#34292,#34293,#34294,#34295,#34296,#34297,#34298,#34299,#34300,#34301,#34302,
#34303,#34304,#34305,#34306,#34307,#34308,#34309,#34310,#34311,#34312,#34313,
#34314,#34315,#34316,#34317,#34318,#34319,#34320,#34321,#34322,#34323,#34324,
#34325,#34326,#34327,#34328,#34329,#34330,#34331,#34332,#34333,#34334,#34335,
#34336,#34337,#34338,#34339,#34340,#34341,#34342,#34343,#34344,#34345,#34346,
#34347,#34348,#34349,#34350,#34351,#34352,#34353,#34354,#34355,#34356,#34357,
#34358,#34359,#34360,#34361,#34362,#34363,#34364,#34365,#34366,#34367,#34368,
#34369,#34370,#34371,#34372,#34373,#34374,#34375,#34376,#34377,#34378,#34379,
#34380,#34381,#34382,#34383,#34384,#34385,#34386,#34387,#34388,#34389,#34390,
#34391,#34392,#34393,#34394,#34395,#34396,#34397,#34398,#34399,#34400,#34401,
#34402,#34403,#34404,#34405,#34406,#34407,#34408,#34409,#34410,#34411,#34412),
(#34413,#34414,#34415,#34416,#34417,#34418,#34419,#34420,#34421,#34422,
#34423,#34424,#34425,#34426,#34427,#34428,#34429,#34430,#34431,#34432,#34433,
#34434,#34435,#34436,#34437,#34438,#34439,#34440,#34441,#34442,#34443,#34444,
#34445,#34446,#34447,#34448,#34449,#34450,#34451,#34452,#34453,#34454,#34455,
#34456,#34457,#34458,#34459,#34460,#34461,#34462,#34463,#34464,#34465,#34466,
#34467,#34468,#34469,#34470,#34471,#34472,#34473,#34474,#34475,#34476,#34477,
#34478,#34479,#34480,#34481,#34482,#34483,#34484,#34485,#34486,#34487,#34488,
#34489,#34490,#34491,#34492,#34493,#34494,#34495,#34496,#34497,#34498,#34499,
#34500,#34501,#34502,#34503,#34504,#34505,#34506,#34507,#34508,#34509,#34510,
#34511,#34512,#34513,#34514,#34515,#34516,#34517,#34518,#34519,#34520,#34521,
#34522,#34523,#34524,#34525,#34526,#34527,#34528,#34529,#34530,#34531,#34532,
#34533,#34534,#34535,#34536,#34537,#34538,#34539,#34540,#34541,#34542,#34543,
#34544,#34545,#34546,#34547,#34548,#34549,#34550,#34551,#34552,#34553,#34554,
#34555,#34556)),.UNSPECIFIED.,.F.,.F.,.F.,(4,4),(4,1,1,1,1,1,1,1,1,1,1,
1,1,1,1,1,1,1,1,1,1,1,1,1,1,1,1,1,1,1,1,1,1,1,1,1,1,1,1,1,1,1,1,1,1,1,1,
1,1,1,1,1,1,1,1,1,1,1,1,1,1,1,1,1,1,1,1,1,1,1,1,1,1,1,1,1,1,1,1,1,1,1,1,
1,1,1,1,1,1,1,1,1,1,1,1,1,1,1,1,1,1,1,1,1,1,1,1,1,1,1,1,1,1,1,1,1,1,1,1,
1,1,1,1,1,1,1,1,1,1,1,1,1,1,1,1,1,1,1,1,1,1,4),(0.,0.0460148164544131),
(8.31058692273977,9.30851679455325,10.3064466663667,11.3043765381802,12.3023064099937,
13.3002362818072,14.2981661536207,15.2960960254341,16.2940258972476,17.2919557690611,
18.2898856408746,19.2878155126881,20.2857453845015,21.283675256315,22.2816051281285,
23.279534999942,24.2774648717555,25.2753947435689,26.2733246153824,27.2712544871959,
28.2691843590094,29.2671142308229,30.2650441026364,31.2629739744498,32.2609038462633,
33.2588337180768,34.2567635898903,35.2546934617038,36.2526233335172,37.2505532053307,
38.2484830771442,39.2464129489577,40.2443428207712,41.2422726925846,42.2402025643981,
43.2381324362116,44.2360623080251,45.2339921798386,46.231922051652,47.2298519234655,
48.227781795279,49.2257116670925,50.223641538906,51.2215714107194,52.2195012825329,
53.2174311543464,54.2153610261599,55.2132908979734,56.2112207697869,57.2091506416003,
58.2070805134138,59.2050103852273,60.2029402570408,61.2008701288543,62.1988000006677,
63.1967298724812,64.1946597442947,65.1925896161082,66.1905194879217,67.1884493597351,
68.1863792315486,69.1843091033621,70.1822389751756,71.1801688469891,72.1780987188026,
73.176028590616,74.1739584624295,75.171888334243,76.1698182060565,77.16774807787,
78.1656779496834,79.1636078214969,80.1615376933104,81.1594675651239,82.1573974369374,
83.1553273087509,84.1532571805643,85.1511870523778,86.1491169241913,87.1470467960048,
88.1449766678183,89.1429065396317,90.1408364114452,91.1387662832587,92.1366961550722,
93.1346260268857,94.1325558986991,95.1304857705126,96.1284156423261,97.1263455141396,
98.1242753859531,99.1222052577666,100.12013512958,101.118065001394,102.115994873207,
103.11392474502,104.111854616834,105.109784488647,106.107714360461,107.105644232274,
108.103574104088,109.101503975901,110.099433847715,111.097363719528,112.095293591342,
113.093223463155,114.091153334969,115.089083206782,116.087013078596,117.084942950409,
118.082872822223,119.080802694036,120.07873256585,121.076662437663,122.074592309477,
123.07252218129,124.070452053104,125.068381924917,126.066311796731,127.064241668544,
128.062171540357,129.060101412171,130.058031283984,131.055961155798,132.053891027611,
133.051820899425,134.049750771238,135.047680643052,136.045610514865,137.043540386679,
138.041470258492,139.039400130306,140.037330002119,141.035259873933,142.033189745746,
143.03111961756,144.029049489373,145.026979361187,146.024909233,147.022839104814,
148.020768976627,149.018698848441),.UNSPECIFIED.);
#507=B_SPLINE_SURFACE_WITH_KNOTS('',3,3,((#34705,#34706,#34707,#34708,#34709,
#34710,#34711,#34712,#34713,#34714,#34715,#34716,#34717,#34718,#34719,#34720,
#34721,#34722,#34723,#34724,#34725,#34726,#34727,#34728,#34729,#34730,#34731,
#34732,#34733,#34734,#34735,#34736,#34737,#34738,#34739,#34740,#34741,#34742,
#34743,#34744,#34745,#34746,#34747,#34748,#34749,#34750,#34751,#34752,#34753,
#34754,#34755,#34756,#34757,#34758,#34759,#34760,#34761,#34762,#34763,#34764,
#34765,#34766,#34767,#34768,#34769,#34770,#34771,#34772,#34773,#34774,#34775,
#34776,#34777,#34778,#34779,#34780,#34781,#34782,#34783,#34784,#34785,#34786,
#34787,#34788,#34789,#34790,#34791,#34792,#34793,#34794,#34795,#34796,#34797,
#34798,#34799,#34800,#34801,#34802,#34803,#34804,#34805,#34806,#34807,#34808,
#34809,#34810,#34811,#34812,#34813,#34814,#34815,#34816,#34817,#34818,#34819,
#34820,#34821,#34822,#34823,#34824,#34825,#34826,#34827,#34828,#34829,#34830,
#34831,#34832,#34833,#34834,#34835,#34836,#34837,#34838,#34839,#34840,#34841,
#34842,#34843,#34844,#34845,#34846,#34847,#34848),(#34849,#34850,#34851,
#34852,#34853,#34854,#34855,#34856,#34857,#34858,#34859,#34860,#34861,#34862,
#34863,#34864,#34865,#34866,#34867,#34868,#34869,#34870,#34871,#34872,#34873,
#34874,#34875,#34876,#34877,#34878,#34879,#34880,#34881,#34882,#34883,#34884,
#34885,#34886,#34887,#34888,#34889,#34890,#34891,#34892,#34893,#34894,#34895,
#34896,#34897,#34898,#34899,#34900,#34901,#34902,#34903,#34904,#34905,#34906,
#34907,#34908,#34909,#34910,#34911,#34912,#34913,#34914,#34915,#34916,#34917,
#34918,#34919,#34920,#34921,#34922,#34923,#34924,#34925,#34926,#34927,#34928,
#34929,#34930,#34931,#34932,#34933,#34934,#34935,#34936,#34937,#34938,#34939,
#34940,#34941,#34942,#34943,#34944,#34945,#34946,#34947,#34948,#34949,#34950,
#34951,#34952,#34953,#34954,#34955,#34956,#34957,#34958,#34959,#34960,#34961,
#34962,#34963,#34964,#34965,#34966,#34967,#34968,#34969,#34970,#34971,#34972,
#34973,#34974,#34975,#34976,#34977,#34978,#34979,#34980,#34981,#34982,#34983,
#34984,#34985,#34986,#34987,#34988,#34989,#34990,#34991,#34992),(#34993,
#34994,#34995,#34996,#34997,#34998,#34999,#35000,#35001,#35002,#35003,#35004,
#35005,#35006,#35007,#35008,#35009,#35010,#35011,#35012,#35013,#35014,#35015,
#35016,#35017,#35018,#35019,#35020,#35021,#35022,#35023,#35024,#35025,#35026,
#35027,#35028,#35029,#35030,#35031,#35032,#35033,#35034,#35035,#35036,#35037,
#35038,#35039,#35040,#35041,#35042,#35043,#35044,#35045,#35046,#35047,#35048,
#35049,#35050,#35051,#35052,#35053,#35054,#35055,#35056,#35057,#35058,#35059,
#35060,#35061,#35062,#35063,#35064,#35065,#35066,#35067,#35068,#35069,#35070,
#35071,#35072,#35073,#35074,#35075,#35076,#35077,#35078,#35079,#35080,#35081,
#35082,#35083,#35084,#35085,#35086,#35087,#35088,#35089,#35090,#35091,#35092,
#35093,#35094,#35095,#35096,#35097,#35098,#35099,#35100,#35101,#35102,#35103,
#35104,#35105,#35106,#35107,#35108,#35109,#35110,#35111,#35112,#35113,#35114,
#35115,#35116,#35117,#35118,#35119,#35120,#35121,#35122,#35123,#35124,#35125,
#35126,#35127,#35128,#35129,#35130,#35131,#35132,#35133,#35134,#35135,#35136),
(#35137,#35138,#35139,#35140,#35141,#35142,#35143,#35144,#35145,#35146,
#35147,#35148,#35149,#35150,#35151,#35152,#35153,#35154,#35155,#35156,#35157,
#35158,#35159,#35160,#35161,#35162,#35163,#35164,#35165,#35166,#35167,#35168,
#35169,#35170,#35171,#35172,#35173,#35174,#35175,#35176,#35177,#35178,#35179,
#35180,#35181,#35182,#35183,#35184,#35185,#35186,#35187,#35188,#35189,#35190,
#35191,#35192,#35193,#35194,#35195,#35196,#35197,#35198,#35199,#35200,#35201,
#35202,#35203,#35204,#35205,#35206,#35207,#35208,#35209,#35210,#35211,#35212,
#35213,#35214,#35215,#35216,#35217,#35218,#35219,#35220,#35221,#35222,#35223,
#35224,#35225,#35226,#35227,#35228,#35229,#35230,#35231,#35232,#35233,#35234,
#35235,#35236,#35237,#35238,#35239,#35240,#35241,#35242,#35243,#35244,#35245,
#35246,#35247,#35248,#35249,#35250,#35251,#35252,#35253,#35254,#35255,#35256,
#35257,#35258,#35259,#35260,#35261,#35262,#35263,#35264,#35265,#35266,#35267,
#35268,#35269,#35270,#35271,#35272,#35273,#35274,#35275,#35276,#35277,#35278,
#35279,#35280)),.UNSPECIFIED.,.F.,.F.,.F.,(4,4),(4,1,1,1,1,1,1,1,1,1,1,
1,1,1,1,1,1,1,1,1,1,1,1,1,1,1,1,1,1,1,1,1,1,1,1,1,1,1,1,1,1,1,1,1,1,1,1,
1,1,1,1,1,1,1,1,1,1,1,1,1,1,1,1,1,1,1,1,1,1,1,1,1,1,1,1,1,1,1,1,1,1,1,1,
1,1,1,1,1,1,1,1,1,1,1,1,1,1,1,1,1,1,1,1,1,1,1,1,1,1,1,1,1,1,1,1,1,1,1,1,
1,1,1,1,1,1,1,1,1,1,1,1,1,1,1,1,1,1,1,1,1,1,4),(0.,0.0460148164544131),
(11.6154215191106,12.6133513909241,13.6112812627376,14.6092111345511,15.6071410063646,
16.605070878178,17.6030007499915,18.600930621805,19.5988604936185,20.596790365432,
21.5947202372454,22.5926501090589,23.5905799808724,24.5885098526859,25.5864397244994,
26.5843695963128,27.5822994681263,28.5802293399398,29.5781592117533,30.5760890835668,
31.5740189553803,32.5719488271937,33.5698786990072,34.5678085708207,35.5657384426342,
36.5636683144477,37.5615981862611,38.5595280580746,39.5574579298881,40.5553878017016,
41.5533176735151,42.5512475453285,43.549177417142,44.5471072889555,45.545037160769,
46.5429670325825,47.540896904396,48.5388267762094,49.5367566480229,50.5346865198364,
51.5326163916499,52.5305462634634,53.5284761352768,54.5264060070903,55.5243358789038,
56.5222657507173,57.5201956225308,58.5181254943442,59.5160553661577,60.5139852379712,
61.5119151097847,62.5098449815982,63.5077748534116,64.5057047252251,65.5036345970386,
66.5015644688521,67.4994943406656,68.497424212479,69.4953540842925,70.493283956106,
71.4912138279195,72.489143699733,73.4870735715464,74.4850034433599,75.4829333151734,
76.4808631869869,77.4787930588004,78.4767229306139,79.4746528024273,80.4725826742408,
81.4705125460543,82.4684424178678,83.4663722896813,84.4643021614947,85.4622320333082,
86.4601619051217,87.4580917769352,88.4560216487487,89.4539515205621,90.4518813923756,
91.4498112641891,92.4477411360026,93.4456710078161,94.4436008796296,95.441530751443,
96.4394606232565,97.43739049507,98.4353203668835,99.433250238697,100.43118011051,
101.429109982324,102.427039854137,103.424969725951,104.422899597764,105.420829469578,
106.418759341391,107.416689213205,108.414619085018,109.412548956832,110.410478828645,
111.408408700459,112.406338572272,113.404268444086,114.402198315899,115.400128187713,
116.398058059526,117.39598793134,118.393917803153,119.391847674967,120.38977754678,
121.387707418594,122.385637290407,123.383567162221,124.381497034034,125.379426905847,
126.377356777661,127.375286649474,128.373216521288,129.371146393101,130.369076264915,
131.367006136728,132.364936008542,133.362865880355,134.360795752169,135.358725623982,
136.356655495796,137.354585367609,138.352515239423,139.350445111236,140.34837498305,
141.346304854863,142.344234726677,143.34216459849,144.340094470304,145.338024342117,
146.335954213931,147.333884085744,148.331813957558,149.329743829371,150.327673701184,
151.325603572998,152.323533444811),.UNSPECIFIED.);
#508=B_SPLINE_SURFACE_WITH_KNOTS('',3,3,((#37042,#37043,#37044,#37045,#37046,
#37047,#37048,#37049,#37050,#37051,#37052,#37053,#37054,#37055,#37056,#37057,
#37058,#37059,#37060,#37061,#37062,#37063,#37064,#37065,#37066,#37067,#37068,
#37069,#37070,#37071,#37072,#37073,#37074,#37075,#37076,#37077,#37078,#37079,
#37080,#37081,#37082,#37083,#37084,#37085,#37086,#37087,#37088,#37089,#37090,
#37091,#37092,#37093,#37094,#37095,#37096,#37097,#37098,#37099,#37100,#37101,
#37102,#37103,#37104,#37105,#37106,#37107,#37108,#37109,#37110,#37111,#37112,
#37113,#37114,#37115,#37116),(#37117,#37118,#37119,#37120,#37121,#37122,
#37123,#37124,#37125,#37126,#37127,#37128,#37129,#37130,#37131,#37132,#37133,
#37134,#37135,#37136,#37137,#37138,#37139,#37140,#37141,#37142,#37143,#37144,
#37145,#37146,#37147,#37148,#37149,#37150,#37151,#37152,#37153,#37154,#37155,
#37156,#37157,#37158,#37159,#37160,#37161,#37162,#37163,#37164,#37165,#37166,
#37167,#37168,#37169,#37170,#37171,#37172,#37173,#37174,#37175,#37176,#37177,
#37178,#37179,#37180,#37181,#37182,#37183,#37184,#37185,#37186,#37187,#37188,
#37189,#37190,#37191),(#37192,#37193,#37194,#37195,#37196,#37197,#37198,
#37199,#37200,#37201,#37202,#37203,#37204,#37205,#37206,#37207,#37208,#37209,
#37210,#37211,#37212,#37213,#37214,#37215,#37216,#37217,#37218,#37219,#37220,
#37221,#37222,#37223,#37224,#37225,#37226,#37227,#37228,#37229,#37230,#37231,
#37232,#37233,#37234,#37235,#37236,#37237,#37238,#37239,#37240,#37241,#37242,
#37243,#37244,#37245,#37246,#37247,#37248,#37249,#37250,#37251,#37252,#37253,
#37254,#37255,#37256,#37257,#37258,#37259,#37260,#37261,#37262,#37263,#37264,
#37265,#37266),(#37267,#37268,#37269,#37270,#37271,#37272,#37273,#37274,
#37275,#37276,#37277,#37278,#37279,#37280,#37281,#37282,#37283,#37284,#37285,
#37286,#37287,#37288,#37289,#37290,#37291,#37292,#37293,#37294,#37295,#37296,
#37297,#37298,#37299,#37300,#37301,#37302,#37303,#37304,#37305,#37306,#37307,
#37308,#37309,#37310,#37311,#37312,#37313,#37314,#37315,#37316,#37317,#37318,
#37319,#37320,#37321,#37322,#37323,#37324,#37325,#37326,#37327,#37328,#37329,
#37330,#37331,#37332,#37333,#37334,#37335,#37336,#37337,#37338,#37339,#37340,
#37341)),.UNSPECIFIED.,.F.,.F.,.F.,(4,4),(4,1,1,1,1,1,1,1,1,1,1,1,1,1,1,
1,1,1,1,1,1,1,1,1,1,1,1,1,1,1,1,1,1,1,1,1,1,1,1,1,1,1,1,1,1,1,1,1,1,1,1,
1,1,1,1,1,1,1,1,1,1,1,1,1,1,1,1,1,1,1,1,1,4),(0.,0.0460148164544132),(8.31058692273973,
9.30493516644425,10.2992834101488,11.2936316538533,12.2879798975578,13.2823281412623,
14.2766763849668,15.2710246286714,16.2653728723759,17.2597211160804,18.2540693597849,
19.2484176034894,20.242765847194,21.2371140908985,22.231462334603,23.2258105783075,
24.220158822012,25.2145070657166,26.2088553094211,27.2032035531256,28.1975517968301,
29.1919000405346,30.1862482842392,31.1805965279437,32.1749447716482,33.1692930153527,
34.1636412590572,35.1579895027618,36.1523377464663,37.1466859901708,38.1410342338753,
39.1353824775798,40.1297307212843,41.1240789649889,42.1184272086934,43.1127754523979,
44.1071236961024,45.1014719398069,46.0958201835115,47.090168427216,48.0845166709205,
49.078864914625,50.0732131583295,51.0675614020341,52.0619096457386,53.0562578894431,
54.0506061331476,55.0449543768521,56.0393026205567,57.0336508642612,58.0279991079657,
59.0223473516702,60.0166955953747,61.0110438390793,62.0053920827838,62.9997403264883,
63.9940885701928,64.9884368138973,65.9827850576018,66.9771333013064,67.9714815450109,
68.9658297887154,69.9601780324199,70.9545262761244,71.948874519829,72.9432227635335,
73.937571007238,74.9319192509425,75.926267494647,76.9206157383516,77.9149639820561,
78.9093122257606,79.9036604694651),.UNSPECIFIED.);
#509=B_SPLINE_SURFACE_WITH_KNOTS('',3,3,((#37549,#37550,#37551,#37552,#37553,
#37554,#37555,#37556,#37557,#37558,#37559,#37560,#37561,#37562,#37563,#37564,
#37565,#37566,#37567,#37568,#37569,#37570,#37571,#37572,#37573,#37574,#37575,
#37576,#37577,#37578,#37579,#37580,#37581,#37582,#37583,#37584,#37585,#37586,
#37587,#37588,#37589,#37590,#37591,#37592,#37593,#37594,#37595,#37596,#37597,
#37598,#37599,#37600,#37601,#37602,#37603,#37604,#37605,#37606,#37607,#37608,
#37609,#37610,#37611,#37612,#37613,#37614,#37615,#37616,#37617,#37618,#37619,
#37620,#37621,#37622,#37623),(#37624,#37625,#37626,#37627,#37628,#37629,
#37630,#37631,#37632,#37633,#37634,#37635,#37636,#37637,#37638,#37639,#37640,
#37641,#37642,#37643,#37644,#37645,#37646,#37647,#37648,#37649,#37650,#37651,
#37652,#37653,#37654,#37655,#37656,#37657,#37658,#37659,#37660,#37661,#37662,
#37663,#37664,#37665,#37666,#37667,#37668,#37669,#37670,#37671,#37672,#37673,
#37674,#37675,#37676,#37677,#37678,#37679,#37680,#37681,#37682,#37683,#37684,
#37685,#37686,#37687,#37688,#37689,#37690,#37691,#37692,#37693,#37694,#37695,
#37696,#37697,#37698),(#37699,#37700,#37701,#37702,#37703,#37704,#37705,
#37706,#37707,#37708,#37709,#37710,#37711,#37712,#37713,#37714,#37715,#37716,
#37717,#37718,#37719,#37720,#37721,#37722,#37723,#37724,#37725,#37726,#37727,
#37728,#37729,#37730,#37731,#37732,#37733,#37734,#37735,#37736,#37737,#37738,
#37739,#37740,#37741,#37742,#37743,#37744,#37745,#37746,#37747,#37748,#37749,
#37750,#37751,#37752,#37753,#37754,#37755,#37756,#37757,#37758,#37759,#37760,
#37761,#37762,#37763,#37764,#37765,#37766,#37767,#37768,#37769,#37770,#37771,
#37772,#37773),(#37774,#37775,#37776,#37777,#37778,#37779,#37780,#37781,
#37782,#37783,#37784,#37785,#37786,#37787,#37788,#37789,#37790,#37791,#37792,
#37793,#37794,#37795,#37796,#37797,#37798,#37799,#37800,#37801,#37802,#37803,
#37804,#37805,#37806,#37807,#37808,#37809,#37810,#37811,#37812,#37813,#37814,
#37815,#37816,#37817,#37818,#37819,#37820,#37821,#37822,#37823,#37824,#37825,
#37826,#37827,#37828,#37829,#37830,#37831,#37832,#37833,#37834,#37835,#37836,
#37837,#37838,#37839,#37840,#37841,#37842,#37843,#37844,#37845,#37846,#37847,
#37848)),.UNSPECIFIED.,.F.,.F.,.F.,(4,4),(4,1,1,1,1,1,1,1,1,1,1,1,1,1,1,
1,1,1,1,1,1,1,1,1,1,1,1,1,1,1,1,1,1,1,1,1,1,1,1,1,1,1,1,1,1,1,1,1,1,1,1,
1,1,1,1,1,1,1,1,1,1,1,1,1,1,1,1,1,1,1,1,1,4),(0.,0.0460148164544132),(11.6154215191106,
12.6097697628151,13.6041180065196,14.5984662502242,15.5928144939287,16.5871627376332,
17.5815109813377,18.5758592250422,19.5702074687467,20.5645557124513,21.5589039561558,
22.5532521998603,23.5476004435648,24.5419486872693,25.5362969309739,26.5306451746784,
27.5249934183829,28.5193416620874,29.5136899057919,30.5080381494965,31.502386393201,
32.4967346369055,33.49108288061,34.4854311243145,35.4797793680191,36.4741276117236,
37.4684758554281,38.4628240991326,39.4571723428371,40.4515205865417,41.4458688302462,
42.4402170739507,43.4345653176552,44.4289135613597,45.4232618050643,46.4176100487688,
47.4119582924733,48.4063065361778,49.4006547798823,50.3950030235868,51.3893512672914,
52.3836995109959,53.3780477547004,54.3723959984049,55.3667442421094,56.361092485814,
57.3554407295185,58.349788973223,59.3441372169275,60.338485460632,61.3328337043366,
62.3271819480411,63.3215301917456,64.3158784354501,65.3102266791546,66.3045749228592,
67.2989231665637,68.2932714102682,69.2876196539727,70.2819678976772,71.2763161413818,
72.2706643850863,73.2650126287908,74.2593608724953,75.2537091161998,76.2480573599044,
77.2424056036089,78.2367538473134,79.2311020910179,80.2254503347224,81.2197985784269,
82.2141468221315,83.208495065836),.UNSPECIFIED.);
#510=B_SPLINE_CURVE_WITH_KNOTS('',3,(#22007,#22008,#22009,#22010,#22011,
#22012,#22013,#22014,#22015,#22016,#22017,#22018,#22019,#22020,#22021,#22022,
#22023,#22024,#22025,#22026,#22027,#22028),.UNSPECIFIED.,.T.,.F.,(4,1,1,
1,1,1,1,1,1,1,1,1,1,1,1,1,1,1,1,4),(-1.23931985388535,-1.15079700717926,
-1.06227416047316,-1.01801273712011,-0.973751313767062,-0.885228467060966,
-0.840967043707917,-0.796705620354869,-0.752444197001821,-0.708182773648772,
-0.619659926942676,-0.531137080236579,-0.486875656883531,-0.442614233530483,
-0.354091386824386,-0.26556854011829,-0.221307116765241,-0.177045693412193,
-0.0885228467060966,0.),.UNSPECIFIED.);
#511=B_SPLINE_CURVE_WITH_KNOTS('',3,(#22120,#22121,#22122,#22123,#22124,
#22125,#22126,#22127),.UNSPECIFIED.,.F.,.F.,(4,1,1,1,1,4),(0.,0.0885228467060966,
0.177045693412193,0.221307116765241,0.26556854011829,0.309829963471338),
 .UNSPECIFIED.);
#512=B_SPLINE_CURVE_WITH_KNOTS('',3,(#22128,#22129,#22130,#22131,#22132,
#22133,#22134,#22135,#22136,#22137,#22138,#22139,#22140,#22141,#22142,#22143,
#22144,#22145),.UNSPECIFIED.,.F.,.F.,(4,1,1,1,1,1,1,1,1,1,1,1,1,1,1,4),
(0.309829963471338,0.354091386824386,0.442614233530483,0.486875656883531,
0.531137080236579,0.619659926942676,0.708182773648772,0.752444197001821,
0.796705620354869,0.840967043707917,0.885228467060966,0.973751313767062,
1.01801273712011,1.06227416047316,1.15079700717926,1.23931985388535),
 .UNSPECIFIED.);
#513=B_SPLINE_CURVE_WITH_KNOTS('',3,(#22150,#22151,#22152,#22153,#22154,
#22155,#22156),.UNSPECIFIED.,.F.,.F.,(4,1,1,1,4),(0.,0.0883566653548034,
0.176713330709607,0.26506999606441,0.309248328741812),.UNSPECIFIED.);
#514=B_SPLINE_CURVE_WITH_KNOTS('',3,(#22157,#22158,#22159,#22160,#22161,
#22162,#22163,#22164,#22165,#22166,#22167,#22168,#22169,#22170,#22171),
 .UNSPECIFIED.,.F.,.F.,(4,1,1,1,1,1,1,1,1,1,1,1,4),(0.309248328741812,0.353426661419213,
0.441783326774017,0.485961659451418,0.53013999212882,0.706853322838427,
0.751031655515829,0.79520998819323,0.883566653548034,0.971923318902837,
1.06027998425764,1.14863664961244,1.23699331496725),.UNSPECIFIED.);
#515=B_SPLINE_CURVE_WITH_KNOTS('',3,(#22483,#22484,#22485,#22486,#22487,
#22488,#22489,#22490,#22491,#22492,#22493,#22494,#22495,#22496,#22497,#22498,
#22499,#22500),.UNSPECIFIED.,.T.,.F.,(4,1,1,1,1,1,1,1,1,1,1,1,1,1,1,4),
(-1.23699331496725,-1.14863664961244,-1.06027998425764,-0.971923318902837,
-0.883566653548034,-0.79520998819323,-0.751031655515829,-0.706853322838427,
-0.53013999212882,-0.485961659451418,-0.441783326774017,-0.353426661419213,
-0.26506999606441,-0.176713330709607,-0.0883566653548034,0.),
 .UNSPECIFIED.);
#516=B_SPLINE_CURVE_WITH_KNOTS('',3,(#22682,#22683,#22684,#22685,#22686,
#22687,#22688,#22689,#22690,#22691),.UNSPECIFIED.,.F.,.F.,(4,2,2,2,4),(0.024631319172959,
0.0777176003976506,0.155435200795301,0.233132476857833,0.310829752920366),
 .UNSPECIFIED.);
#517=B_SPLINE_CURVE_WITH_KNOTS('',3,(#22695,#22696,#22697,#22698,#22699,
#22700,#22701,#22702,#22703,#22704),.UNSPECIFIED.,.F.,.F.,(4,2,2,2,4),(0.932489258761097,
1.01018653482363,1.08788381088616,1.16560141128381,1.2186876925085),
 .UNSPECIFIED.);
#518=B_SPLINE_CURVE_WITH_KNOTS('',3,(#22707,#22708,#22709,#22710,#22711,
#22712,#22713,#22714,#22715,#22716),.UNSPECIFIED.,.F.,.F.,(4,2,2,2,4),(0.64629082501369,
0.699377106238382,0.777094706636032,0.854791982698564,0.932489258761097),
 .UNSPECIFIED.);
#519=B_SPLINE_CURVE_WITH_KNOTS('',3,(#22719,#22720,#22721,#22722,#22723,
#22724,#22725,#22726,#22727,#22728),.UNSPECIFIED.,.F.,.F.,(4,2,2,2,4),(0.310829752920366,
0.388527028982898,0.46622430504543,0.54394190544308,0.597028186667772),
 .UNSPECIFIED.);
#520=B_SPLINE_CURVE_WITH_KNOTS('',3,(#22741,#22742,#22743,#22744,#22745,
#22746,#22747,#22748,#22749,#22750,#22751,#22752,#22753,#22754,#22755,#22756,
#22757,#22758,#22759,#22760,#22761,#22762,#22763,#22764,#22765,#22766),
 .UNSPECIFIED.,.F.,.F.,(4,2,2,2,2,2,2,2,2,2,2,2,4),(0.,0.0773604855652864,
0.154720971130573,0.232079805418848,0.309438639707124,0.3867974739954,0.464156308283676,
0.541516793848962,0.618877279414249,0.696237764979535,0.773598250544821,
0.850957084833097,0.928315919121373),.UNSPECIFIED.);
#521=B_SPLINE_CURVE_WITH_KNOTS('',3,(#22767,#22768,#22769,#22770,#22771,
#22772,#22773,#22774,#22775,#22776),.UNSPECIFIED.,.F.,.F.,(4,2,2,2,4),(0.928315919121373,
1.00567475340965,1.08303358769792,1.16039407326321,1.2377545588285),
 .UNSPECIFIED.);
#522=B_SPLINE_CURVE_WITH_KNOTS('',3,(#22786,#22787,#22788,#22789,#22790,
#22791,#22792,#22793,#22794,#22795),.UNSPECIFIED.,.F.,.F.,(4,2,2,2,4),(0.,
0.0773604855652864,0.154720971130573,0.232079805418848,0.309438639707124),
 .UNSPECIFIED.);
#523=B_SPLINE_CURVE_WITH_KNOTS('',3,(#22797,#22798,#22799,#22800,#22801,
#22802,#22803,#22804,#22805,#22806),.UNSPECIFIED.,.F.,.F.,(4,2,2,2,4),(0.928315919121373,
1.00567475340965,1.08303358769792,1.16039407326321,1.2377545588285),
 .UNSPECIFIED.);
#524=B_SPLINE_CURVE_WITH_KNOTS('',3,(#22807,#22808,#22809,#22810,#22811,
#22812,#22813,#22814,#22815,#22816,#22817,#22818,#22819,#22820,#22821,#22822,
#22823,#22824),.UNSPECIFIED.,.F.,.F.,(4,2,2,2,2,2,2,2,4),(0.309438639707124,
0.3867974739954,0.464156308283676,0.541516793848962,0.618877279414249,0.696237764979535,
0.773598250544821,0.850957084833097,0.928315919121373),.UNSPECIFIED.);
#525=B_SPLINE_CURVE_WITH_KNOTS('',3,(#22834,#22835,#22836,#22837,#22838,
#22839,#22840,#22841,#22842,#22843),.UNSPECIFIED.,.F.,.F.,(4,2,2,2,4),(0.0246313191729586,
0.0777176003976506,0.155435200795301,0.233132476857833,0.310829752920366),
 .UNSPECIFIED.);
#526=B_SPLINE_CURVE_WITH_KNOTS('',3,(#22846,#22847,#22848,#22849,#22850,
#22851,#22852,#22853,#22854,#22855,#22856,#22857,#22858,#22859,#22860,#22861,
#22862,#22863),.UNSPECIFIED.,.F.,.F.,(4,2,2,2,2,2,2,2,4),(0.64629082501369,
0.699377106238382,0.777094706636033,0.854791982698565,0.932489258761097,
1.01018653482363,1.08788381088616,1.16560141128381,1.2186876925085),
 .UNSPECIFIED.);
#527=B_SPLINE_CURVE_WITH_KNOTS('',3,(#22864,#22865,#22866,#22867,#22868,
#22869,#22870,#22871,#22872,#22873),.UNSPECIFIED.,.F.,.F.,(4,2,2,2,4),(0.310829752920366,
0.388527028982898,0.46622430504543,0.543941905443081,0.597028186667773),
 .UNSPECIFIED.);
#528=B_SPLINE_CURVE_WITH_KNOTS('',3,(#23411,#23412,#23413,#23414,#23415,
#23416,#23417,#23418,#23419,#23420,#23421,#23422,#23423,#23424,#23425,#23426,
#23427,#23428,#23429,#23430,#23431,#23432,#23433,#23434,#23435,#23436,#23437,
#23438,#23439,#23440,#23441,#23442,#23443,#23444,#23445,#23446,#23447,#23448,
#23449,#23450,#23451,#23452,#23453),.UNSPECIFIED.,.F.,.F.,(4,3,3,3,3,3,
3,3,3,3,3,3,3,3,4),(-10.3761157273102,-10.2282534190556,-9.75949053544433,
-9.29072765183303,-8.82196476822174,-8.35320188461044,-7.88443900099915,
-7.41567611738786,-6.94691323377656,-6.47815035016526,-6.00938746655397,
-5.54062458294268,-5.07186169933138,-4.60309881572009,-4.16739290401597),
 .UNSPECIFIED.);
#529=B_SPLINE_CURVE_WITH_KNOTS('',3,(#23456,#23457,#23458,#23459,#23460,
#23461,#23462,#23463,#23464,#23465,#23466,#23467,#23468,#23469,#23470,#23471,
#23472,#23473,#23474,#23475,#23476,#23477,#23478,#23479,#23480,#23481,#23482,
#23483,#23484,#23485,#23486,#23487,#23488,#23489,#23490,#23491,#23492,#23493,
#23494,#23495,#23496,#23497,#23498),.UNSPECIFIED.,.F.,.F.,(4,3,3,3,3,3,
3,3,3,3,3,3,3,3,4),(1.20264568843901,1.67491189387389,2.14717809930877,
2.61944430474366,3.09171051017854,3.56397671561342,4.03624292104831,4.50850912648319,
4.98077533191807,5.45304153735295,5.92530774278784,6.39757394822272,6.8698401536576,
7.34210635909249,7.41136851173327),.UNSPECIFIED.);
#530=B_SPLINE_CURVE_WITH_KNOTS('',3,(#23503,#23504,#23505,#23506,#23507,
#23508,#23509,#23510,#23511,#23512,#23513,#23514,#23515,#23516,#23517,#23518,
#23519,#23520,#23521,#23522,#23523,#23524,#23525,#23526,#23527,#23528,#23529,
#23530,#23531,#23532,#23533,#23534,#23535,#23536,#23537,#23538,#23539,#23540,
#23541,#23542,#23543,#23544,#23545),.UNSPECIFIED.,.F.,.F.,(4,3,3,3,3,3,
3,3,3,3,3,3,3,3,4),(-16.6593010344898,-16.3221709060024,-15.8534080223912,
-15.3846451387799,-14.9158822551686,-14.4471193715573,-13.978356487946,
-13.5095936043347,-13.0408307207234,-12.5720678371121,-12.1033049535008,
-11.6345420698895,-11.1657791862782,-10.6970163026669,-10.3761157273102),
 .UNSPECIFIED.);
#531=B_SPLINE_CURVE_WITH_KNOTS('',3,(#23546,#23547,#23548,#23549,#23550,
#23551,#23552,#23553,#23554,#23555,#23556,#23557,#23558,#23559,#23560,#23561,
#23562,#23563,#23564,#23565,#23566,#23567,#23568,#23569,#23570,#23571,#23572,
#23573,#23574,#23575,#23576,#23577,#23578,#23579,#23580,#23581,#23582,#23583,
#23584,#23585,#23586,#23587,#23588),.UNSPECIFIED.,.F.,.F.,(4,3,3,3,3,3,
3,3,3,3,3,3,3,3,4),(7.41136851173327,7.81437256452737,8.28663876996226,
8.75890497539714,9.23117118083202,9.7034373862669,10.1757035917018,10.6479697971367,
11.1202360025716,11.5925022080064,12.0647684134413,12.5370346188762,13.0093008243111,
13.481567029746,13.6945538189129),.UNSPECIFIED.);
#532=B_SPLINE_CURVE_WITH_KNOTS('',3,(#23594,#23595,#23596,#23597,#23598,
#23599,#23600,#23601,#23602,#23603,#23604,#23605,#23606,#23607),
 .UNSPECIFIED.,.F.,.F.,(4,1,1,1,1,1,1,1,1,1,1,4),(21.9911485751285,22.3120491504852,
22.7808120340965,23.2495749177078,23.7183378013191,24.1871006849304,24.6558635685417,
25.124626452153,25.5933893357643,26.0621522193756,26.5309151029869,26.7952085499488),
 .UNSPECIFIED.);
#533=B_SPLINE_CURVE_WITH_KNOTS('',3,(#23610,#23611,#23612,#23613,#23614,
#23615,#23616,#23617,#23618,#23619,#23620),.UNSPECIFIED.,.F.,.F.,(4,1,1,
1,1,1,1,1,4),(21.9911485751285,22.2504279913965,22.7226941968314,23.1949604022663,
23.6672266077012,24.1394928131361,24.611759018571,25.0840252240059,25.5562914294407),
 .UNSPECIFIED.);
#534=B_SPLINE_CURVE_WITH_KNOTS('',3,(#23627,#23628,#23629,#23630,#23631,
#23632,#23633,#23634,#23635,#23636,#23637,#23638,#23639,#23640,#23641,#23642,
#23643),.UNSPECIFIED.,.F.,.F.,(4,1,1,1,1,1,1,1,1,1,1,1,1,1,4),(15.7493687799271,
16.2181316635384,16.6868945471497,17.155657430761,17.6244203143723,18.0931831979836,
18.5619460815949,19.0307089652062,19.4994718488175,19.9682347324288,20.4369976160401,
20.9057604996514,21.3745233832627,21.8432862668739,21.9911485751285),
 .UNSPECIFIED.);
#535=B_SPLINE_CURVE_WITH_KNOTS('',3,(#23644,#23645,#23646,#23647,#23648,
#23649,#23650,#23651,#23652,#23653,#23654,#23655,#23656,#23657,#23658,#23659,
#23660),.UNSPECIFIED.,.F.,.F.,(4,1,1,1,1,1,1,1,1,1,1,1,1,1,4),(15.707963267949,
16.1109673207431,16.583233526178,17.0554997316128,17.5277659370477,18.0000321424826,
18.4722983479175,18.9445645533524,19.4168307587873,19.8890969642221,20.361363169657,
20.8336293750919,21.3058955805268,21.7781617859617,21.9911485751285),
 .UNSPECIFIED.);
#536=B_SPLINE_CURVE_WITH_KNOTS('',3,(#23811,#23812,#23813,#23814,#23815,
#23816),.UNSPECIFIED.,.F.,.F.,(4,2,4),(0.00194275133685398,0.0331760695218423,
0.0663555691945392),.UNSPECIFIED.);
#537=B_SPLINE_CURVE_WITH_KNOTS('',3,(#23818,#23819,#23820,#23821,#23822,
#23823,#23824),.UNSPECIFIED.,.F.,.F.,(4,3,4),(0.0503544158881505,0.216395299739162,
0.250849009142881),.UNSPECIFIED.);
#538=B_SPLINE_CURVE_WITH_KNOTS('',3,(#23826,#23827,#23828,#23829,#23830,
#23831),.UNSPECIFIED.,.F.,.F.,(4,2,4),(0.,0.0331528039224116,0.0596005631617877),
 .UNSPECIFIED.);
#539=B_SPLINE_CURVE_WITH_KNOTS('',3,(#23832,#23833,#23834,#23835,#23836,
#23837,#23838,#23839,#23840,#23841,#23842),.UNSPECIFIED.,.F.,.F.,(4,1,1,
1,1,1,1,1,4),(12.644156658622,12.8051038826989,13.2773700881338,13.7496362935687,
14.2219024990035,14.6941687044384,15.1664349098733,15.6387011153082,15.707963267949),
 .UNSPECIFIED.);
#540=B_SPLINE_CURVE_WITH_KNOTS('',3,(#23844,#23845,#23846,#23847,#23848,
#23849,#23850,#23851,#23852,#23853,#23854,#23855,#23856,#23857,#23858,#23859,
#23860,#23861,#23862,#23863,#23864,#23865,#23866,#23867,#23868,#23869,#23870,
#23871,#23872,#23873,#23874,#23875,#23876,#23877,#23878,#23879,#23880,#23881,
#23882,#23883,#23884,#23885,#23886,#23887,#23888,#23889,#23890,#23891,#23892,
#23893,#23894,#23895,#23896,#23897,#23898,#23899,#23900,#23901,#23902,#23903,
#23904,#23905,#23906,#23907,#23908,#23909,#23910,#23911,#23912,#23913,#23914,
#23915,#23916,#23917,#23918,#23919,#23920,#23921,#23922,#23923,#23924,#23925),
 .UNSPECIFIED.,.F.,.F.,(4,3,3,3,3,3,3,3,3,3,3,3,3,3,3,3,3,3,3,3,3,3,3,3,
3,3,3,4),(-2.74250302776518,-2.57686990184093,-2.48672838486568,-2.42438465251614,
-2.38771591000872,-2.22247456456748,-2.11726591049527,-2.05259329034323,
-2.02076827609199,-1.85670314451872,-1.69196748309613,-1.57688547236148,
-1.53552332264269,-1.50624221680821,-1.3425714308067,-1.23163944015751,
-1.07689892021046,-1.03296271663657,-0.9930706972102,-0.830572896985994,
-0.668873173603195,-0.612677360369303,-0.533465071065458,-0.502301898288595,
-0.34107686385133,-0.179301278866167,-0.0205350393876634,0.),
 .UNSPECIFIED.);
#541=B_SPLINE_CURVE_WITH_KNOTS('',3,(#23926,#23927,#23928,#23929,#23930,
#23931,#23932,#23933,#23934,#23935,#23936,#23937,#23938),.UNSPECIFIED.,
 .F.,.F.,(4,3,3,3,4),(13.6945538189129,13.9538332351809,14.4260994406157,
14.8983656460506,15.1801757021305),.UNSPECIFIED.);
#542=B_SPLINE_CURVE_WITH_KNOTS('',3,(#23940,#23941,#23942,#23943,#23944,
#23945),.UNSPECIFIED.,.F.,.F.,(4,2,4),(0.0278987519445973,0.0331528039168248,
0.0663033314332046),.UNSPECIFIED.);
#543=B_SPLINE_CURVE_WITH_KNOTS('',3,(#23947,#23948,#23949,#23950,#23951,
#23952,#23953,#23954,#23955,#23956,#23957,#23958,#23959,#23960,#23961,#23962,
#23963,#23964,#23965,#23966,#23967,#23968,#23969,#23970,#23971,#23972,#23973,
#23974,#23975,#23976,#23977,#23978,#23979,#23980),.UNSPECIFIED.,.F.,.F.,
(4,3,3,3,3,3,3,3,3,3,3,4),(-2.7450049110565,-2.58394001349979,-2.45527459604387,
-2.40771262127862,-2.37283567347439,-2.22079245860333,-2.1259413782344,
-2.07191392018567,-2.04033511913998,-1.8778682623923,-1.71515635324971,
-1.60487049281501),.UNSPECIFIED.);
#544=B_SPLINE_CURVE_WITH_KNOTS('',3,(#23981,#23982,#23983,#23984,#23985,
#23986,#23987,#23988,#23989),.UNSPECIFIED.,.F.,.F.,(4,1,1,1,1,1,4),(10.3761157273102,
10.4437728555245,10.9160390609594,11.3883052663942,11.8605714718291,12.332837677264,
12.4885845700963),.UNSPECIFIED.);
#545=B_SPLINE_CURVE_WITH_KNOTS('',3,(#23996,#23997,#23998,#23999,#24000,
#24001,#24002,#24003,#24004,#24005,#24006,#24007,#24008,#24009,#24010,#24011,
#24012,#24013,#24014,#24015,#24016,#24017,#24018,#24019,#24020,#24021,#24022,
#24023,#24024,#24025,#24026,#24027,#24028,#24029,#24030,#24031,#24032,#24033,
#24034,#24035,#24036,#24037,#24038),.UNSPECIFIED.,.F.,.F.,(4,3,3,3,3,3,
3,3,3,3,3,3,3,3,4),(-2.74250302776508,-2.66850832126571,-2.50265052845,
-2.39214152203743,-2.35757539427899,-2.19175335172764,-2.08902158205883,
-2.04611352983189,-2.01171973266703,-1.84702980906273,-1.78082627305242,
-1.61618310024309,-1.53556392179723,-1.50606805204129,-1.3410808692064),
 .UNSPECIFIED.);
#546=B_SPLINE_CURVE_WITH_KNOTS('',3,(#24047,#24048,#24049,#24050,#24051,
#24052,#24053,#24054,#24055,#24056,#24057,#24058,#24059,#24060,#24061,#24062,
#24063,#24064,#24065,#24066,#24067,#24068,#24069,#24070,#24071,#24072,#24073,
#24074,#24075,#24076,#24077,#24078,#24079,#24080),.UNSPECIFIED.,.F.,.F.,
(4,3,3,3,3,3,3,3,3,3,3,4),(-1.14003686198146,-1.05830319525406,-1.0207818545891,
-0.992096849082759,-0.829622775007598,-0.666879442976059,-0.576523485569153,
-0.520860847165652,-0.486167528162247,-0.325408793834023,-0.162704396917011,
0.),.UNSPECIFIED.);
#547=B_SPLINE_CURVE_WITH_KNOTS('',3,(#24087,#24088,#24089,#24090,#24091,
#24092,#24093,#24094,#24095,#24096,#24097,#24098,#24099,#24100,#24101,#24102,
#24103,#24104,#24105,#24106,#24107,#24108,#24109,#24110,#24111,#24112,#24113,
#24114,#24115,#24116,#24117,#24118,#24119,#24120),.UNSPECIFIED.,.F.,.F.,
(4,3,3,3,3,3,3,3,3,3,3,4),(-1.40414311178045,-1.24106650608481,-1.10748442566693,
-1.06335789746563,-1.02152275246228,-0.856189859529963,-0.706738184413317,
-0.541595540057656,-0.502301503557962,-0.336744830409687,-0.168372415204844,
0.),.UNSPECIFIED.);
#548=B_SPLINE_CURVE_WITH_KNOTS('',3,(#24247,#24248,#24249,#24250,#24251,
#24252),.UNSPECIFIED.,.F.,.F.,(4,2,4),(0.,0.0331760695065475,0.0651963829308363),
 .UNSPECIFIED.);
#549=B_SPLINE_CURVE_WITH_KNOTS('',3,(#24254,#24255,#24256,#24257,#24258,
#24259,#24260),.UNSPECIFIED.,.F.,.F.,(4,3,4),(-17.259696673225,-16.7909337896137,
-16.6593010344898),.UNSPECIFIED.);
#550=B_SPLINE_CURVE_WITH_KNOTS('',3,(#24261,#24262,#24263,#24264,#24265,
#24266,#24267,#24268,#24269,#24270,#24271,#24272,#24273,#24274,#24275,#24276,
#24277,#24278,#24279,#24280,#24281,#24282,#24283,#24284,#24285,#24286,#24287,
#24288,#24289,#24290,#24291,#24292,#24293,#24294,#24295,#24296,#24297,#24298,
#24299,#24300,#24301,#24302,#24303,#24304,#24305,#24306,#24307,#24308,#24309,
#24310,#24311,#24312,#24313,#24314,#24315,#24316,#24317,#24318,#24319,#24320,
#24321,#24322,#24323,#24324,#24325,#24326,#24327,#24328,#24329,#24330,#24331,
#24332,#24333,#24334,#24335,#24336,#24337,#24338,#24339,#24340,#24341,#24342),
 .UNSPECIFIED.,.F.,.F.,(4,3,3,3,3,3,3,3,3,3,3,3,3,3,3,3,3,3,3,3,3,3,3,3,
3,3,3,4),(-2.74500491105659,-2.58350402394403,-2.48061289382144,-2.41107509153194,
-2.37265853925204,-2.21067382092066,-2.12552001520103,-2.08101176042865,
-2.04586716316976,-1.88271537722459,-1.87005859804212,-1.7095303618963,
-1.59527874414824,-1.55981736007669,-1.52718746411221,-1.36294474918432,
-1.25252389090405,-1.09667110605016,-1.05462433202708,-1.02403188127795,
-0.859632450592286,-0.694838694901999,-0.629112751488469,-0.545267156057735,
-0.502057707499426,-0.336851513025011,-0.168425756512506,0.),
 .UNSPECIFIED.);
#551=B_SPLINE_CURVE_WITH_KNOTS('',3,(#24343,#24344,#24345,#24346),
 .UNSPECIFIED.,.F.,.F.,(4,4),(0.0501531527093442,0.0969267489892359),
 .UNSPECIFIED.);
#552=B_SPLINE_CURVE_WITH_KNOTS('',3,(#24384,#24385,#24386,#24387),
 .UNSPECIFIED.,.F.,.F.,(4,4),(0.0335690789016969,0.0663555691090524),
 .UNSPECIFIED.);
#553=B_SPLINE_CURVE_WITH_KNOTS('',3,(#24389,#24390,#24391,#24392,#24393,
#24394,#24395,#24396,#24397,#24398,#24399,#24400,#24401),.UNSPECIFIED.,
 .F.,.F.,(4,3,3,3,4),(-4.01846793624531,-3.68613209857994,-3.02146042324921,
-2.35678874791848,-2.07952097109452),.UNSPECIFIED.);
#554=B_SPLINE_CURVE_WITH_KNOTS('',3,(#24403,#24404,#24405,#24406,#24407,
#24408),.UNSPECIFIED.,.F.,.F.,(4,2,4),(0.,0.0331528039173847,0.0663033314433819),
 .UNSPECIFIED.);
#555=B_SPLINE_CURVE_WITH_KNOTS('',3,(#24409,#24410,#24411,#24412,#24413,
#24414,#24415,#24416,#24417),.UNSPECIFIED.,.F.,.F.,(4,1,1,1,1,1,4),(12.644156658622,
12.9748140827407,13.6394857580714,13.9718215957368,14.6364932710675,15.3011649463983,
15.6301772236861),.UNSPECIFIED.);
#556=B_SPLINE_CURVE_WITH_KNOTS('',3,(#24439,#24440,#24441,#24442),
 .UNSPECIFIED.,.F.,.F.,(4,4),(0.,0.0278987520022068),.UNSPECIFIED.);
#557=B_SPLINE_CURVE_WITH_KNOTS('',3,(#24443,#24444,#24445,#24446,#24447),
 .UNSPECIFIED.,.F.,.F.,(4,1,4),(11.6150328478183,11.9900267092154,12.4885845700963),
 .UNSPECIFIED.);
#558=B_SPLINE_CURVE_WITH_KNOTS('',3,(#24480,#24481,#24482,#24483,#24484,
#24485),.UNSPECIFIED.,.F.,.F.,(4,2,4),(0.,0.0331760694937226,0.0335690788757423),
 .UNSPECIFIED.);
#559=B_SPLINE_CURVE_WITH_KNOTS('',3,(#24486,#24487,#24488,#24489,#24490,
#24491,#24492),.UNSPECIFIED.,.F.,.F.,(4,3,4),(0.,0.52686036033418,1.05372072066836),
 .UNSPECIFIED.);
#560=B_SPLINE_CURVE_WITH_KNOTS('',3,(#24587,#24588,#24589,#24590,#24591,
#24592,#24593,#24594,#24595,#24596),.UNSPECIFIED.,.F.,.F.,(4,3,3,4),(-4.09254174883832,
-3.94657662118458,-2.95993246588844,-2.06514013327811),.UNSPECIFIED.);
#561=B_SPLINE_CURVE_WITH_KNOTS('',3,(#24599,#24600,#24601,#24602,#24603,
#24604,#24605),.UNSPECIFIED.,.F.,.F.,(4,3,4),(0.,0.986644155296146,1.11419103802958),
 .UNSPECIFIED.);
#562=B_SPLINE_CURVE_WITH_KNOTS('',3,(#24610,#24611,#24612,#24613,#24614,
#24615,#24616,#24617,#24618,#24619,#24620,#24621,#24622,#24623,#24624,#24625,
#24626,#24627,#24628,#24629,#24630,#24631),.UNSPECIFIED.,.F.,.F.,(4,3,3,
3,3,3,3,4),(-10.3757270560179,-9.86644155296145,-8.87979739766531,-7.89315324236916,
-6.90650908707302,-5.91986493177687,-4.93322077648073,-4.09254174883832),
 .UNSPECIFIED.);
#563=B_SPLINE_CURVE_WITH_KNOTS('',3,(#24632,#24633,#24634,#24635,#24636,
#24637,#24638,#24639,#24640,#24641,#24642,#24643,#24644,#24645,#24646,#24647,
#24648,#24649,#24650,#24651,#24652,#24653),.UNSPECIFIED.,.F.,.F.,(4,3,3,
3,3,3,3,4),(1.11419103802958,1.97328831059229,2.95993246588844,3.94657662118458,
4.93322077648073,5.91986493177687,6.90650908707302,7.39737634520917),
 .UNSPECIFIED.);
#564=B_SPLINE_CURVE_WITH_KNOTS('',3,(#24658,#24659,#24660,#24661,#24662,
#24663,#24664,#24665,#24666,#24667,#24668,#24669,#24670,#24671,#24672,#24673,
#24674,#24675,#24676,#24677,#24678,#24679),.UNSPECIFIED.,.F.,.F.,(4,3,3,
3,3,3,3,4),(-16.6589123631975,-15.7863064847383,-14.7996623294422,-13.813018174146,
-12.8263740188499,-11.8397298635537,-10.8530857082576,-10.3757270560179),
 .UNSPECIFIED.);
#565=B_SPLINE_CURVE_WITH_KNOTS('',3,(#24680,#24681,#24682,#24683,#24684,
#24685,#24686,#24687,#24688,#24689,#24690,#24691,#24692,#24693,#24694,#24695,
#24696,#24697,#24698,#24699,#24700,#24701),.UNSPECIFIED.,.F.,.F.,(4,3,3,
3,3,3,3,4),(7.39737634520917,7.89315324236916,8.87979739766531,9.86644155296146,
10.8530857082576,11.8397298635537,12.8263740188499,13.6805616523888),
 .UNSPECIFIED.);
#566=B_SPLINE_CURVE_WITH_KNOTS('',3,(#24706,#24707,#24708,#24709,#24710,
#24711,#24712,#24713,#24714,#24715,#24716,#24717,#24718,#24719,#24720,#24721,
#24722,#24723,#24724,#24725,#24726,#24727,#24728,#24729,#24730),
 .UNSPECIFIED.,.F.,.F.,(4,3,3,3,3,3,3,3,4),(-22.9420976703771,-22.6928155718113,
-21.7061714165152,-20.719527261219,-19.7328831059229,-18.7462389506268,
-17.7595947953306,-16.7729506400345,-16.6589123631975),.UNSPECIFIED.);
#567=B_SPLINE_CURVE_WITH_KNOTS('',3,(#24731,#24732,#24733,#24734,#24735,
#24736,#24737,#24738,#24739,#24740,#24741,#24742,#24743,#24744,#24745,#24746,
#24747,#24748,#24749,#24750,#24751,#24752,#24753,#24754,#24755),
 .UNSPECIFIED.,.F.,.F.,(4,3,3,3,3,3,3,3,4),(13.6805616523888,13.813018174146,
14.7996623294422,15.7863064847383,16.7729506400345,17.7595947953306,18.7462389506268,
19.7328831059229,19.9637469595683),.UNSPECIFIED.);
#568=B_SPLINE_CURVE_WITH_KNOTS('',3,(#24760,#24761,#24762,#24763,#24764,
#24765,#24766,#24767,#24768,#24769,#24770,#24771,#24772,#24773,#24774,#24775,
#24776,#24777,#24778,#24779,#24780,#24781),.UNSPECIFIED.,.F.,.F.,(4,3,3,
3,3,3,3,4),(-29.2252829775567,-28.6126805035882,-27.6260363482921,-26.6393921929959,
-25.6527480376998,-24.6661038824036,-23.6794597271075,-22.9420976703771),
 .UNSPECIFIED.);
#569=B_SPLINE_CURVE_WITH_KNOTS('',3,(#24782,#24783,#24784,#24785,#24786,
#24787,#24788,#24789,#24790,#24791,#24792,#24793,#24794,#24795,#24796,#24797,
#24798,#24799,#24800,#24801,#24802,#24803),.UNSPECIFIED.,.F.,.F.,(4,3,3,
3,3,3,3,4),(19.9637469595683,20.719527261219,21.7061714165152,22.6928155718113,
23.6794597271075,24.6661038824036,25.6527480376998,26.2469322667479),
 .UNSPECIFIED.);
#570=B_SPLINE_CURVE_WITH_KNOTS('',3,(#24808,#24809,#24810,#24811,#24812,
#24813,#24814,#24815,#24816,#24817,#24818,#24819,#24820,#24821,#24822,#24823,
#24824,#24825,#24826,#24827,#24828,#24829),.UNSPECIFIED.,.F.,.F.,(4,3,3,
3,3,3,3,4),(-35.5084682847363,-34.5325454353651,-33.5459012800689,-32.5592571247728,
-31.5726129694767,-30.5859688141805,-29.5993246588844,-29.2252829775567),
 .UNSPECIFIED.);
#571=B_SPLINE_CURVE_WITH_KNOTS('',3,(#24830,#24831,#24832,#24833,#24834,
#24835,#24836,#24837,#24838,#24839,#24840,#24841,#24842,#24843,#24844,#24845,
#24846,#24847,#24848,#24849,#24850,#24851),.UNSPECIFIED.,.F.,.F.,(4,3,3,
3,3,3,3,4),(26.2469322667479,26.6393921929959,27.6260363482921,28.6126805035882,
29.5993246588844,30.5859688141805,31.5726129694767,32.5301175739275),
 .UNSPECIFIED.);
#572=B_SPLINE_CURVE_WITH_KNOTS('',3,(#24857,#24858,#24859,#24860,#24861,
#24862,#24863),.UNSPECIFIED.,.F.,.F.,(4,1,1,1,4),(47.1238898038469,47.1346111097719,
48.121255265068,49.1078994203642,50.0026917529745),.UNSPECIFIED.);
#573=B_SPLINE_CURVE_WITH_KNOTS('',3,(#24866,#24867,#24868,#24869,#24870),
 .UNSPECIFIED.,.F.,.F.,(4,1,4),(47.1238898038469,47.7763531345856,48.7629972898817),
 .UNSPECIFIED.);
#574=B_SPLINE_CURVE_WITH_KNOTS('',3,(#24875,#24876,#24877,#24878,#24879,
#24880,#24881,#24882,#24883,#24884),.UNSPECIFIED.,.F.,.F.,(4,1,1,1,1,1,
1,4),(40.8407044966673,41.214746177995,42.2013903332911,43.1880344885873,
44.1746786438834,45.1613227991796,46.1479669544757,47.1238898038469),
 .UNSPECIFIED.);
#575=B_SPLINE_CURVE_WITH_KNOTS('',3,(#24885,#24886,#24887,#24888,#24889,
#24890,#24891,#24892,#24893,#24894,#24895),.UNSPECIFIED.,.F.,.F.,(4,1,1,
1,1,1,1,1,4),(40.8407044966673,40.8698440475126,41.8564882028087,42.8431323581049,
43.829776513401,44.8164206686971,45.8030648239933,46.7897089792894,47.1238898038469),
 .UNSPECIFIED.);
#576=B_SPLINE_CURVE_WITH_KNOTS('',3,(#24900,#24901,#24902,#24903,#24904,
#24905,#24906,#24907,#24908,#24909),.UNSPECIFIED.,.F.,.F.,(4,1,1,1,1,1,
1,4),(34.5575191894877,35.2948812462181,36.2815254015143,37.2681695568104,
38.2548137121066,39.2414578674027,40.2281020226988,40.8407044966673),
 .UNSPECIFIED.);
#577=B_SPLINE_CURVE_WITH_KNOTS('',3,(#24910,#24911,#24912,#24913,#24914,
#24915,#24916,#24917,#24918,#24919),.UNSPECIFIED.,.F.,.F.,(4,1,1,1,1,1,
1,4),(34.5575191894877,34.9499791157357,35.9366232710318,36.923267426328,
37.9099115816241,38.8965557369203,39.8831998922164,40.8407044966673),
 .UNSPECIFIED.);
#578=B_SPLINE_CURVE_WITH_KNOTS('',3,(#24924,#24925,#24926,#24927,#24928,
#24929,#24930,#24931,#24932,#24933,#24934),.UNSPECIFIED.,.F.,.F.,(4,1,1,
1,1,1,1,1,4),(28.2743338823081,28.3883721591451,29.3750163144413,30.3616604697374,
31.3483046250335,32.3349487803297,33.3215929356258,34.308237090922,34.5575191894877),
 .UNSPECIFIED.);
#579=B_SPLINE_CURVE_WITH_KNOTS('',3,(#24935,#24936,#24937,#24938,#24939,
#24940,#24941,#24942,#24943,#24944),.UNSPECIFIED.,.F.,.F.,(4,1,1,1,1,1,
1,4),(28.2743338823081,29.0301141839588,30.016758339255,31.0034024945511,
31.9900466498473,32.9766908051434,33.9633349604396,34.5575191894877),
 .UNSPECIFIED.);
#580=B_SPLINE_CURVE_WITH_KNOTS('',3,(#24949,#24950,#24951,#24952,#24953,
#24954,#24955,#24956,#24957,#24958),.UNSPECIFIED.,.F.,.F.,(4,1,1,1,1,1,
1,4),(21.9911485751285,22.4685072273682,23.4551513826644,24.4417955379605,
25.4284396932567,26.4150838485528,27.401728003849,28.2743338823081),
 .UNSPECIFIED.);
#581=B_SPLINE_CURVE_WITH_KNOTS('',3,(#24959,#24960,#24961,#24962,#24963,
#24964,#24965,#24966,#24967,#24968,#24969),.UNSPECIFIED.,.F.,.F.,(4,1,1,
1,1,1,1,1,4),(21.9911485751285,22.1236050968858,23.110249252182,24.0968934074781,
25.0835375627742,26.0701817180704,27.0568258733665,28.0434700286627,28.2743338823081),
 .UNSPECIFIED.);
#582=B_SPLINE_CURVE_WITH_KNOTS('',3,(#24974,#24975,#24976,#24977,#24978,
#24979,#24980,#24981,#24982,#24983),.UNSPECIFIED.,.F.,.F.,(4,1,1,1,1,1,
1,4),(15.707963267949,16.5486422955914,17.5352864508875,18.5219306061837,
19.5085747614798,20.4952189167759,21.4818630720721,21.9911485751285),
 .UNSPECIFIED.);
#583=B_SPLINE_CURVE_WITH_KNOTS('',3,(#24984,#24985,#24986,#24987,#24988,
#24989,#24990,#24991,#24992,#24993),.UNSPECIFIED.,.F.,.F.,(4,1,1,1,1,1,
1,4),(15.7079632679489,16.2037401651089,17.1903843204051,18.1770284757012,
19.1636726309974,20.1503167862935,21.1369609415897,21.9911485751285),
 .UNSPECIFIED.);
#584=B_SPLINE_CURVE_WITH_KNOTS('',3,(#24996,#24997,#24998,#24999,#25000,
#25001,#25002,#25003,#25004,#25005,#25006,#25007,#25008,#25009,#25010,#25011,
#25012,#25013,#25014,#25015,#25016,#25017,#25018,#25019,#25020,#25021,#25022,
#25023,#25024,#25025,#25026,#25027,#25028,#25029,#25030,#25031,#25032,#25033,
#25034,#25035,#25036,#25037,#25038,#25039,#25040,#25041,#25042,#25043,#25044,
#25045,#25046,#25047),.UNSPECIFIED.,.F.,.F.,(4,3,3,3,3,3,3,3,3,3,3,3,3,
3,3,3,3,4),(-0.366397579005847,-0.351842688178875,-0.332838158855069,-0.315678481693382,
-0.289420321645097,-0.273011785342624,-0.237897749313856,-0.221715923866805,
-0.207723971026893,-0.185180840167277,-0.161636550067305,-0.147128811889025,
-0.135731814711402,-0.101798861033552,-0.076880688176872,-0.0670092782892109,
-0.0285139790106868,0.),.UNSPECIFIED.);
#585=B_SPLINE_CURVE_WITH_KNOTS('',3,(#25052,#25053,#25054,#25055,#25056,
#25057,#25058,#25059,#25060,#25061,#25062,#25063,#25064,#25065,#25066,#25067,
#25068,#25069,#25070,#25071,#25072,#25073,#25074,#25075,#25076,#25077,#25078,
#25079,#25080,#25081,#25082,#25083,#25084,#25085,#25086,#25087,#25088,#25089,
#25090,#25091,#25092,#25093,#25094,#25095,#25096,#25097,#25098,#25099,#25100,
#25101,#25102,#25103,#25104,#25105,#25106),.UNSPECIFIED.,.F.,.F.,(4,3,3,
3,3,3,3,3,3,3,3,3,3,3,3,3,3,3,4),(-0.364629307890685,-0.346730130939237,
-0.318258076668756,-0.304671300367645,-0.283283926727407,-0.268750032662776,
-0.256211185988777,-0.219678588916904,-0.20148985221534,-0.1862389075973,
-0.164290383513372,-0.139072476943319,-0.127435374126706,-0.116240718055298,
-0.0871805385414733,-0.0683502117761216,-0.0546744719449251,-0.022336513706662,
0.),.UNSPECIFIED.);
#586=B_SPLINE_CURVE_WITH_KNOTS('',3,(#25283,#25284,#25285,#25286,#25287,
#25288,#25289,#25290,#25291,#25292,#25293,#25294,#25295,#25296,#25297,#25298,
#25299,#25300,#25301,#25302,#25303,#25304),.UNSPECIFIED.,.F.,.F.,(4,3,3,
3,3,3,3,4),(32.5301175739275,32.5592571247728,33.5459012800689,34.5325454353651,
35.5191895906612,36.5058337459574,37.4924779012535,38.3872702338639),
 .UNSPECIFIED.);
#587=B_SPLINE_CURVE_WITH_KNOTS('',3,(#25306,#25307,#25308,#25309,#25310,
#25311,#25312,#25313,#25314,#25315,#25316,#25317,#25318,#25319,#25320,#25321,
#25322,#25323,#25324,#25325,#25326,#25327,#25328,#25329,#25330,#25331,#25332,
#25333,#25334,#25335,#25336,#25337,#25338,#25339,#25340,#25341,#25342,#25343,
#25344,#25345,#25346,#25347,#25348,#25349,#25350,#25351,#25352,#25353,#25354,
#25355,#25356,#25357),.UNSPECIFIED.,.F.,.F.,(4,3,3,3,3,3,3,3,3,3,3,3,3,
3,3,3,3,4),(-0.36639757900584,-0.351842688178868,-0.332838163030847,-0.315678486081905,
-0.289414746484995,-0.273012692426124,-0.237898677161377,-0.221717024761523,
-0.207724021339265,-0.18518084016727,-0.161636547239729,-0.147128781690345,
-0.135731805846515,-0.101798854384886,-0.0768806612204703,-0.0670092358876265,
-0.0285139219945927,0.),.UNSPECIFIED.);
#588=B_SPLINE_CURVE_WITH_KNOTS('',3,(#25358,#25359,#25360,#25361,#25362,
#25363,#25364,#25365,#25366),.UNSPECIFIED.,.F.,.F.,(4,1,1,1,1,1,4),(10.3757270560179,
11.2705193886282,12.2571635439244,13.2438076992205,14.2304518545166,15.2170960098128,
15.7079632679489),.UNSPECIFIED.);
#589=B_SPLINE_CURVE_WITH_KNOTS('',3,(#25372,#25373,#25374,#25375,#25376,
#25377,#25378,#25379,#25380,#25381,#25382,#25383,#25384,#25385,#25386,#25387,
#25388,#25389,#25390,#25391,#25392,#25393,#25394,#25395,#25396,#25397,#25398,
#25399,#25400,#25401,#25402,#25403,#25404,#25405,#25406,#25407,#25408,#25409,
#25410,#25411,#25412,#25413,#25414,#25415,#25416,#25417,#25418,#25419,#25420,
#25421,#25422,#25423,#25424,#25425,#25426),.UNSPECIFIED.,.F.,.F.,(4,3,3,
3,3,3,3,3,3,3,3,3,3,3,3,3,3,3,4),(-0.36462930789067,-0.346730130939223,
-0.318258061840929,-0.304671288555113,-0.283283871503023,-0.268749409502959,
-0.256211230718671,-0.219678613621225,-0.201489854814136,-0.186238903270344,
-0.164290383513369,-0.139072549937506,-0.127435742460392,-0.116240765389693,
-0.0871805740422699,-0.0683502946375612,-0.0546744738896406,-0.0223365680991636,
0.),.UNSPECIFIED.);
#590=B_SPLINE_CURVE_WITH_KNOTS('',3,(#25429,#25430,#25431,#25432,#25433,
#25434,#25435,#25436),.UNSPECIFIED.,.F.,.F.,(4,1,1,1,1,4),(11.6154215191106,
12.6020656744068,13.5887098297029,14.5753539849991,15.5619981402952,15.707963267949),
 .UNSPECIFIED.);
#591=B_SPLINE_CURVE_WITH_KNOTS('',3,(#25613,#25614,#25615,#25616,#25617,
#25618,#25619,#25620,#25621,#25622,#25623,#25624,#25625,#25626,#25627,#25628,
#25629,#25630,#25631),.UNSPECIFIED.,.F.,.F.,(4,3,3,3,3,3,4),(-40.452410367142,
-39.4657662118458,-38.4791220565497,-37.4924779012535,-36.5058337459574,
-35.5191895906612,-35.5084682847363),.UNSPECIFIED.);
#592=B_SPLINE_CURVE_WITH_KNOTS('',3,(#25799,#25800,#25801,#25802,#25803,
#25804,#25805,#25806,#25807,#25808),.UNSPECIFIED.,.F.,.F.,(4,3,3,4),(-4.09254174883832,
-3.93455391961068,-2.95091543970801,-2.06514013327811),.UNSPECIFIED.);
#593=B_SPLINE_CURVE_WITH_KNOTS('',3,(#25811,#25812,#25813,#25814,#25815,
#25816,#25817),.UNSPECIFIED.,.F.,.F.,(4,3,4),(0.,0.983638479902673,1.11419103802959),
 .UNSPECIFIED.);
#594=B_SPLINE_CURVE_WITH_KNOTS('',3,(#25822,#25823,#25824,#25825,#25826,
#25827,#25828,#25829,#25830,#25831,#25832,#25833,#25834,#25835,#25836,#25837,
#25838,#25839,#25840,#25841,#25842,#25843),.UNSPECIFIED.,.F.,.F.,(4,3,3,
3,3,3,3,4),(-10.3757270560179,-9.83638479902669,-8.85274631912402,-7.86910783922136,
-6.88546935931869,-5.90183087941602,-4.91819239951335,-4.09254174883832),
 .UNSPECIFIED.);
#595=B_SPLINE_CURVE_WITH_KNOTS('',3,(#25844,#25845,#25846,#25847,#25848,
#25849,#25850,#25851,#25852,#25853,#25854,#25855,#25856,#25857,#25858,#25859,
#25860,#25861,#25862,#25863,#25864,#25865),.UNSPECIFIED.,.F.,.F.,(4,3,3,
3,3,3,3,4),(1.11419103802959,1.96727695980534,2.95091543970801,3.93455391961068,
4.91819239951335,5.90183087941602,6.88546935931869,7.39737634520918),
 .UNSPECIFIED.);
#596=B_SPLINE_CURVE_WITH_KNOTS('',3,(#25870,#25871,#25872,#25873,#25874,
#25875,#25876,#25877,#25878,#25879,#25880,#25881,#25882,#25883,#25884,#25885,
#25886,#25887,#25888,#25889,#25890,#25891),.UNSPECIFIED.,.F.,.F.,(4,3,3,
3,3,3,3,4),(-16.6589123631975,-15.7382156784427,-14.75457719854,-13.7709387186374,
-12.7873002387347,-11.803661758832,-10.8200232789294,-10.3757270560179),
 .UNSPECIFIED.);
#597=B_SPLINE_CURVE_WITH_KNOTS('',3,(#25892,#25893,#25894,#25895,#25896,
#25897,#25898,#25899,#25900,#25901,#25902,#25903,#25904,#25905,#25906,#25907,
#25908,#25909,#25910,#25911,#25912,#25913),.UNSPECIFIED.,.F.,.F.,(4,3,3,
3,3,3,3,4),(7.39737634520918,7.86910783922136,8.85274631912403,9.83638479902669,
10.8200232789294,11.803661758832,12.7873002387347,13.6805616523888),
 .UNSPECIFIED.);
#598=B_SPLINE_CURVE_WITH_KNOTS('',3,(#25918,#25919,#25920,#25921,#25922,
#25923,#25924,#25925,#25926,#25927,#25928,#25929,#25930,#25931,#25932,#25933,
#25934,#25935,#25936,#25937,#25938,#25939,#25940,#25941,#25942),
 .UNSPECIFIED.,.F.,.F.,(4,3,3,3,3,3,3,3,4),(-22.9420976703771,-22.6236850377614,
-21.6400465578587,-20.6564080779561,-19.6727695980534,-18.6891311181507,
-17.705492638248,-16.7218541583454,-16.6589123631975),.UNSPECIFIED.);
#599=B_SPLINE_CURVE_WITH_KNOTS('',3,(#25943,#25944,#25945,#25946,#25947,
#25948,#25949,#25950,#25951,#25952,#25953,#25954,#25955,#25956,#25957,#25958,
#25959,#25960,#25961,#25962,#25963,#25964,#25965,#25966,#25967),
 .UNSPECIFIED.,.F.,.F.,(4,3,3,3,3,3,3,3,4),(13.6805616523888,13.7709387186374,
14.75457719854,15.7382156784427,16.7218541583454,17.705492638248,18.6891311181507,
19.6727695980534,19.9637469595684),.UNSPECIFIED.);
#600=B_SPLINE_CURVE_WITH_KNOTS('',3,(#25972,#25973,#25974,#25975,#25976,
#25977,#25978,#25979,#25980,#25981,#25982,#25983,#25984,#25985,#25986,#25987,
#25988,#25989,#25990,#25991,#25992,#25993),.UNSPECIFIED.,.F.,.F.,(4,3,3,
3,3,3,3,4),(-29.2252829775567,-28.5255159171774,-27.5418774372747,-26.5582389573721,
-25.5746004774694,-24.5909619975667,-23.6073235176641,-22.9420976703771),
 .UNSPECIFIED.);
#601=B_SPLINE_CURVE_WITH_KNOTS('',3,(#25994,#25995,#25996,#25997,#25998,
#25999,#26000,#26001,#26002,#26003,#26004,#26005,#26006,#26007,#26008,#26009,
#26010,#26011,#26012,#26013,#26014,#26015),.UNSPECIFIED.,.F.,.F.,(4,3,3,
3,3,3,3,4),(19.9637469595684,20.6564080779561,21.6400465578587,22.6236850377614,
23.6073235176641,24.5909619975667,25.5746004774694,26.2469322667479),
 .UNSPECIFIED.);
#602=B_SPLINE_CURVE_WITH_KNOTS('',3,(#26021,#26022,#26023,#26024),
 .UNSPECIFIED.,.F.,.F.,(4,4),(40.8407044966673,41.026712742718),
 .UNSPECIFIED.);
#603=B_SPLINE_CURVE_WITH_KNOTS('',3,(#26030,#26031,#26032,#26033,#26034,
#26035,#26036,#26037,#26038,#26039),.UNSPECIFIED.,.F.,.F.,(4,1,1,1,1,1,
1,4),(34.5575191894877,35.2227450367747,36.2063835166774,37.19002199658,
38.1736604764827,39.1572989563854,40.1409374362881,40.8407044966673),
 .UNSPECIFIED.);
#604=B_SPLINE_CURVE_WITH_KNOTS('',3,(#26042,#26043,#26044,#26045,#26046,
#26047,#26048,#26049,#26050),.UNSPECIFIED.,.F.,.F.,(4,1,1,1,1,1,4),(34.5575191894877,
34.8688258801119,35.8524643600145,36.8361028399172,37.8197413198199,38.8033797997225,
39.7870182796252),.UNSPECIFIED.);
#605=B_SPLINE_CURVE_WITH_KNOTS('',3,(#26055,#26056,#26057,#26058,#26059,
#26060,#26061,#26062,#26063,#26064,#26065),.UNSPECIFIED.,.F.,.F.,(4,1,1,
1,1,1,1,1,4),(28.2743338823081,28.337275677456,29.3209141573587,30.3045526372614,
31.288191117164,32.2718295970667,33.2554680769694,34.239106556872,34.5575191894877),
 .UNSPECIFIED.);
#606=B_SPLINE_CURVE_WITH_KNOTS('',3,(#26066,#26067,#26068,#26069,#26070,
#26071,#26072,#26073,#26074,#26075),.UNSPECIFIED.,.F.,.F.,(4,1,1,1,1,1,
1,4),(28.2743338823081,28.9669950006958,29.9506334805985,30.9342719605012,
31.9179104404039,32.9015489203065,33.8851874002092,34.5575191894877),
 .UNSPECIFIED.);
#607=B_SPLINE_CURVE_WITH_KNOTS('',3,(#26080,#26081,#26082,#26083,#26084,
#26085,#26086,#26087,#26088,#26089),.UNSPECIFIED.,.F.,.F.,(4,1,1,1,1,1,
1,4),(21.9911485751285,22.43544479804,23.4190832779427,24.4027217578453,
25.386360237748,26.3699987176507,27.3536371975534,28.2743338823081),
 .UNSPECIFIED.);
#608=B_SPLINE_CURVE_WITH_KNOTS('',3,(#26090,#26091,#26092,#26093,#26094,
#26095,#26096,#26097,#26098,#26099,#26100),.UNSPECIFIED.,.F.,.F.,(4,1,1,
1,1,1,1,1,4),(21.9911485751285,22.0815256413772,23.0651641212798,24.0488026011825,
25.0324410810852,26.0160795609878,26.9997180408905,27.9833565207932,28.2743338823081),
 .UNSPECIFIED.);
#609=B_SPLINE_CURVE_WITH_KNOTS('',3,(#26105,#26106,#26107,#26108,#26109,
#26110,#26111,#26112,#26113,#26114),.UNSPECIFIED.,.F.,.F.,(4,1,1,1,1,1,
1,4),(15.707963267949,16.533613918624,17.5172523985267,18.5008908784293,
19.484529358332,20.4681678382347,21.4518063181373,21.9911485751285),
 .UNSPECIFIED.);
#610=B_SPLINE_CURVE_WITH_KNOTS('',3,(#26115,#26116,#26117,#26118,#26119,
#26120,#26121,#26122,#26123,#26124),.UNSPECIFIED.,.F.,.F.,(4,1,1,1,1,1,
1,4),(15.707963267949,16.1796947619611,17.1633332418638,18.1469717217665,
19.1306102016691,20.1142486815718,21.0978871614745,21.9911485751285),
 .UNSPECIFIED.);
#611=B_SPLINE_CURVE_WITH_KNOTS('',3,(#26127,#26128,#26129,#26130,#26131,
#26132,#26133,#26134,#26135,#26136,#26137,#26138,#26139,#26140,#26141,#26142,
#26143,#26144,#26145,#26146,#26147,#26148,#26149,#26150,#26151,#26152,#26153,
#26154,#26155,#26156,#26157,#26158,#26159,#26160,#26161,#26162,#26163,#26164,
#26165,#26166,#26167,#26168,#26169,#26170,#26171,#26172,#26173,#26174,#26175,
#26176,#26177,#26178),.UNSPECIFIED.,.F.,.F.,(4,3,3,3,3,3,3,3,3,3,3,3,3,
3,3,3,3,4),(-0.366397579005848,-0.350883706971702,-0.330766239349036,-0.315517000142461,
-0.286726965402577,-0.272902702918689,-0.237792065049709,-0.221751325260965,
-0.207725190445974,-0.184643803987141,-0.160983363133761,-0.147813025816132,
-0.137069449159236,-0.102802086869427,-0.0797357051045986,-0.0678496931522027,
-0.0293463862030034,0.),.UNSPECIFIED.);
#612=B_SPLINE_CURVE_WITH_KNOTS('',3,(#26183,#26184,#26185,#26186,#26187,
#26188,#26189,#26190,#26191,#26192,#26193,#26194,#26195,#26196,#26197,#26198,
#26199,#26200,#26201,#26202,#26203,#26204,#26205,#26206,#26207,#26208,#26209,
#26210,#26211,#26212,#26213,#26214,#26215,#26216,#26217,#26218,#26219,#26220,
#26221,#26222,#26223,#26224,#26225,#26226,#26227,#26228,#26229,#26230,#26231,
#26232,#26233,#26234,#26235,#26236,#26237),.UNSPECIFIED.,.F.,.F.,(4,3,3,
3,3,3,3,3,3,3,3,3,3,3,3,3,3,3,4),(-0.364629307890673,-0.34556327172486,
-0.316373806239452,-0.304392727635835,-0.282581484008551,-0.264372375760159,
-0.252241992724549,-0.215817384559742,-0.198585804821849,-0.187223821335194,
-0.163761333129925,-0.14297227179632,-0.127520914102002,-0.116250236265464,
-0.0871876771990984,-0.0683674864494023,-0.0546742414735358,-0.0223329481946053,
0.),.UNSPECIFIED.);
#613=B_SPLINE_CURVE_WITH_KNOTS('',3,(#26378,#26379,#26380,#26381,#26382,
#26383,#26384,#26385,#26386,#26387,#26388,#26389,#26390),.UNSPECIFIED.,
 .F.,.F.,(4,3,3,3,4),(26.2469322667479,26.5582389573721,27.5418774372747,
28.5255159171774,29.4112912236073),.UNSPECIFIED.);
#614=B_SPLINE_CURVE_WITH_KNOTS('',3,(#26392,#26393,#26394,#26395,#26396,
#26397,#26398,#26399,#26400,#26401,#26402,#26403,#26404,#26405,#26406,#26407,
#26408,#26409,#26410,#26411,#26412,#26413,#26414,#26415,#26416,#26417,#26418,
#26419,#26420,#26421,#26422,#26423,#26424,#26425,#26426,#26427,#26428,#26429,
#26430,#26431,#26432,#26433,#26434,#26435,#26436,#26437,#26438,#26439,#26440,
#26441,#26442,#26443),.UNSPECIFIED.,.F.,.F.,(4,3,3,3,3,3,3,3,3,3,3,3,3,
3,3,3,3,4),(-0.366397579005841,-0.350883706971692,-0.330766244233555,-0.315517008906463,
-0.286727928129561,-0.272902925597775,-0.237792297289449,-0.221751641342226,
-0.207725209589122,-0.184643803987137,-0.160983359465905,-0.147812972159593,
-0.137069363910321,-0.102802022932741,-0.0797355322205692,-0.0678497129848781,
-0.0293463878428536,0.),.UNSPECIFIED.);
#615=B_SPLINE_CURVE_WITH_KNOTS('',3,(#26444,#26445,#26446,#26447,#26448,
#26449,#26450,#26451,#26452),.UNSPECIFIED.,.F.,.F.,(4,1,1,1,1,1,4),(10.3757270560179,
11.2615023624478,12.2451408423505,13.2287793222531,14.2124178021558,15.1960562820585,
15.707963267949),.UNSPECIFIED.);
#616=B_SPLINE_CURVE_WITH_KNOTS('',3,(#26458,#26459,#26460,#26461,#26462,
#26463,#26464,#26465,#26466,#26467,#26468,#26469,#26470,#26471,#26472,#26473,
#26474,#26475,#26476,#26477,#26478,#26479,#26480,#26481,#26482,#26483,#26484,
#26485,#26486,#26487,#26488,#26489,#26490,#26491,#26492,#26493,#26494,#26495,
#26496,#26497,#26498,#26499,#26500,#26501,#26502,#26503,#26504,#26505,#26506,
#26507,#26508,#26509,#26510,#26511,#26512),.UNSPECIFIED.,.F.,.F.,(4,3,3,
3,3,3,3,3,3,3,3,3,3,3,3,3,3,3,4),(-0.364629307890667,-0.345563271724857,
-0.316373785930453,-0.304392687069709,-0.282581361533379,-0.264370838693491,
-0.252241562212899,-0.215816938962755,-0.198585271532288,-0.18722386611403,
-0.163761333129928,-0.142972181196261,-0.127520768604021,-0.116250225520689,
-0.087187669140517,-0.0683674708033287,-0.0546742449026845,-0.0223330177554359,
0.),.UNSPECIFIED.);
#617=B_SPLINE_CURVE_WITH_KNOTS('',3,(#26515,#26516,#26517,#26518,#26519,
#26520,#26521,#26522),.UNSPECIFIED.,.F.,.F.,(4,1,1,1,1,4),(11.6154215191106,
12.5990599990133,13.582698478916,14.5663369588187,15.5499754387213,15.707963267949),
 .UNSPECIFIED.);
#618=B_SPLINE_CURVE_WITH_KNOTS('',3,(#26663,#26664,#26665,#26666,#26667,
#26668,#26669,#26670,#26671,#26672),.UNSPECIFIED.,.F.,.F.,(4,3,3,4),(-31.4764313568854,
-30.4927928769827,-29.5091543970801,-29.2252829775567),.UNSPECIFIED.);
#619=B_SPLINE_CURVE_WITH_KNOTS('',3,(#27021,#27022,#27023,#27024,#27025,
#27026,#27027,#27028,#27029,#27030,#27031,#27032,#27033,#27034,#27035,#27036,
#27037,#27038,#27039,#27040,#27041,#27042,#27043,#27044),.UNSPECIFIED.,
 .F.,.F.,(4,1,1,1,1,1,1,1,2,2,2,2,1,1,1,1,1,4),(0.,0.0483649312414982,0.0967298624829964,
0.145094793724495,0.193459724965993,0.241824656207491,0.290189587448989,
0.326463285880113,0.386919449931986,0.464302426118159,0.541687686804892,
0.619072947491625,0.677110750756395,0.735148554021165,0.793186357285935,
0.851224160550705,0.909261963815475,0.928609421237438),.UNSPECIFIED.);
#620=B_SPLINE_CURVE_WITH_KNOTS('',3,(#27045,#27046,#27047,#27048,#27049,
#27050,#27051,#27052,#27053,#27054),.UNSPECIFIED.,.F.,.F.,(4,1,1,2,2,4),
(0.928609421237438,0.967299767080245,0.99631866871263,1.08337537360978,
1.16076063429652,1.23814589498325),.UNSPECIFIED.);
#621=B_SPLINE_CURVE_WITH_KNOTS('',3,(#27055,#27056,#27057,#27058,#27059,
#27060,#27061,#27062,#27063,#27064,#27065,#27066,#27067,#27068,#27069,#27070,
#27071,#27072,#27073,#27074,#27075,#27076,#27077,#27078,#27079,#27080,#27081,
#27082,#27083,#27084),.UNSPECIFIED.,.T.,.F.,(4,2,2,1,1,1,1,1,1,1,2,2,2,
2,1,1,1,1,1,1,1,4),(-1.23814589498325,-1.16076063429652,-1.08337537360978,
-0.99631866871263,-0.967299767080245,-0.909261963815475,-0.851224160550705,
-0.793186357285935,-0.735148554021165,-0.677110750756395,-0.619072947491625,
-0.541687686804892,-0.464302426118159,-0.386919449931986,-0.326463285880113,
-0.290189587448989,-0.241824656207491,-0.193459724965993,-0.145094793724495,
-0.0967298624829964,-0.0483649312414982,0.),.UNSPECIFIED.);
#622=B_SPLINE_CURVE_WITH_KNOTS('',3,(#27097,#27098,#27099,#27100,#27101,
#27102,#27103,#27104,#27105,#27106,#27107,#27108,#27109,#27110,#27111,#27112),
 .UNSPECIFIED.,.F.,.F.,(4,2,2,2,2,2,1,1,4),(0.358934429201528,0.49197868985962,
0.564785636730508,0.596617469546802,0.699442998635822,0.77716819339067,
0.842568141080894,0.907968088771118,0.932576705821461),.UNSPECIFIED.);
#623=B_SPLINE_CURVE_WITH_KNOTS('',3,(#27113,#27114,#27115,#27116,#27117,
#27118,#27119,#27120,#27121,#27122,#27123,#27124,#27125,#27126),
 .UNSPECIFIED.,.F.,.F.,(4,1,1,1,1,1,2,2,1,4),(0.932576705821461,0.973368036461342,
1.03876798415157,1.07146795799668,1.10416793184179,1.16956787953201,1.30036777491246,
1.39600843428647,1.50005496459849,1.6041014949105),.UNSPECIFIED.);
#624=B_SPLINE_CURVE_WITH_KNOTS('',3,(#27253,#27254,#27255,#27256,#27257,
#27258,#27259,#27260,#27261,#27262),.UNSPECIFIED.,.F.,.F.,(4,1,2,2,1,4),
(-1.6041014949105,-1.50005496459849,-1.39600843428647,-1.30036777491246,
-1.16956787953201,-1.14109494863627),.UNSPECIFIED.);
#625=B_SPLINE_CURVE_WITH_KNOTS('',3,(#27264,#27265,#27266,#27267,#27268,
#27269,#27270,#27271,#27272,#27273,#27274,#27275),.UNSPECIFIED.,.F.,.F.,
(4,1,1,1,1,1,1,2,4),(-1.14109494863627,-1.10416793184179,-1.07146795799668,
-1.03876798415157,-0.973368036461342,-0.907968088771118,-0.842568141080894,
-0.77716819339067,-0.72405846300665),.UNSPECIFIED.);
#626=B_SPLINE_CURVE_WITH_KNOTS('',3,(#27276,#27277,#27278,#27279,#27280,
#27281,#27282,#27283,#27284,#27285,#27286,#27287),.UNSPECIFIED.,.F.,.F.,
(4,2,2,2,2,4),(-0.72405846300665,-0.699442998635822,-0.596617469546802,
-0.564785636730508,-0.49197868985962,-0.358934429201528),.UNSPECIFIED.);
#627=B_SPLINE_CURVE_WITH_KNOTS('',3,(#27590,#27591,#27592,#27593,#27594,
#27595,#27596,#27597,#27598,#27599),.UNSPECIFIED.,.F.,.F.,(4,3,3,4),(-4.09274904019421,
-3.98125488127007,-2.98594116095255,-2.07317267331972),.UNSPECIFIED.);
#628=B_SPLINE_CURVE_WITH_KNOTS('',3,(#27602,#27603,#27604,#27605,#27606,
#27607,#27608),.UNSPECIFIED.,.F.,.F.,(4,3,4),(0.,0.995313720317508,1.12201628671524),
 .UNSPECIFIED.);
#629=B_SPLINE_CURVE_WITH_KNOTS('',3,(#27613,#27614,#27615,#27616,#27617,
#27618,#27619,#27620,#27621,#27622,#27623,#27624,#27625,#27626,#27627,#27628,
#27629,#27630,#27631,#27632,#27633,#27634),.UNSPECIFIED.,.F.,.F.,(4,3,3,
3,3,3,3,4),(-10.3759343473738,-9.95313720317518,-8.95782348285766,-7.96250976254015,
-6.96719604222263,-5.97188232190511,-4.9765686015876,-4.09274904019421),
 .UNSPECIFIED.);
#630=B_SPLINE_CURVE_WITH_KNOTS('',3,(#27635,#27636,#27637,#27638,#27639,
#27640,#27641,#27642,#27643,#27644,#27645,#27646,#27647,#27648,#27649,#27650,
#27651,#27652,#27653,#27654,#27655,#27656),.UNSPECIFIED.,.F.,.F.,(4,3,3,
3,3,3,3,4),(1.12201628671524,1.99062744063502,2.98594116095254,3.98125488127006,
4.97656860158758,5.9718823219051,6.96719604222262,7.40520159389483),
 .UNSPECIFIED.);
#631=B_SPLINE_CURVE_WITH_KNOTS('',3,(#27661,#27662,#27663,#27664,#27665,
#27666,#27667,#27668,#27669,#27670,#27671,#27672,#27673,#27674,#27675,#27676,
#27677,#27678,#27679,#27680,#27681,#27682),.UNSPECIFIED.,.F.,.F.,(4,3,3,
3,3,3,3,4),(-16.6591196545534,-15.9250195250803,-14.9297058047628,-13.9343920844453,
-12.9390783641277,-11.9437646438102,-10.9484509234927,-10.3759343473738),
 .UNSPECIFIED.);
#632=B_SPLINE_CURVE_WITH_KNOTS('',3,(#27683,#27684,#27685,#27686,#27687,
#27688,#27689,#27690,#27691,#27692,#27693,#27694,#27695,#27696,#27697,#27698,
#27699,#27700,#27701,#27702,#27703,#27704),.UNSPECIFIED.,.F.,.F.,(4,3,3,
3,3,3,3,4),(7.40520159389483,7.96250976254014,8.95782348285766,9.95313720317518,
10.9484509234927,11.9437646438102,12.9390783641277,13.6883869010744),
 .UNSPECIFIED.);
#633=B_SPLINE_CURVE_WITH_KNOTS('',3,(#27709,#27710,#27711,#27712,#27713,
#27714,#27715,#27716,#27717,#27718,#27719,#27720,#27721,#27722,#27723,#27724,
#27725,#27726,#27727,#27728,#27729,#27730,#27731,#27732,#27733),
 .UNSPECIFIED.,.F.,.F.,(4,3,3,3,3,3,3,3,4),(-22.942304961733,-22.8922155673029,
-21.8969018469854,-20.9015881266679,-19.9062744063504,-18.9109606860328,
-17.9156469657153,-16.9203332453978,-16.6591196545534),.UNSPECIFIED.);
#634=B_SPLINE_CURVE_WITH_KNOTS('',3,(#27734,#27735,#27736,#27737,#27738,
#27739,#27740,#27741,#27742,#27743,#27744,#27745,#27746,#27747,#27748,#27749,
#27750,#27751,#27752,#27753,#27754,#27755,#27756,#27757,#27758),
 .UNSPECIFIED.,.F.,.F.,(4,3,3,3,3,3,3,3,4),(13.6883869010744,13.9343920844453,
14.9297058047628,15.9250195250803,16.9203332453978,17.9156469657153,18.9109606860329,
19.9062744063504,19.971572208254),.UNSPECIFIED.);
#635=B_SPLINE_CURVE_WITH_KNOTS('',3,(#27763,#27764,#27765,#27766,#27767,
#27768,#27769,#27770,#27771,#27772,#27773,#27774,#27775,#27776,#27777,#27778,
#27779,#27780,#27781,#27782,#27783,#27784),.UNSPECIFIED.,.F.,.F.,(4,3,3,
3,3,3,3,4),(-29.2254902689126,-28.864097889208,-27.8687841688905,-26.873470448573,
-25.8781567282555,-24.882843007938,-23.8875292876204,-22.942304961733),
 .UNSPECIFIED.);
#636=B_SPLINE_CURVE_WITH_KNOTS('',3,(#27785,#27786,#27787,#27788,#27789,
#27790,#27791,#27792,#27793,#27794,#27795,#27796,#27797,#27798,#27799,#27800,
#27801,#27802,#27803,#27804,#27805,#27806),.UNSPECIFIED.,.F.,.F.,(4,3,3,
3,3,3,3,4),(19.971572208254,20.9015881266679,21.8969018469854,22.8922155673029,
23.8875292876204,24.882843007938,25.8781567282555,26.2547575154336),
 .UNSPECIFIED.);
#637=B_SPLINE_CURVE_WITH_KNOTS('',3,(#27811,#27812,#27813,#27814,#27815,
#27816,#27817,#27818,#27819,#27820,#27821,#27822,#27823,#27824,#27825,#27826,
#27827,#27828,#27829,#27830,#27831,#27832),.UNSPECIFIED.,.F.,.F.,(4,3,3,
3,3,3,3,4),(-35.5086755760921,-34.8359802111131,-33.8406664907956,-32.8453527704781,
-31.8500390501606,-30.8547253298431,-29.8594116095255,-29.2254902689126),
 .UNSPECIFIED.);
#638=B_SPLINE_CURVE_WITH_KNOTS('',3,(#27833,#27834,#27835,#27836,#27837,
#27838,#27839,#27840,#27841,#27842,#27843,#27844,#27845,#27846,#27847,#27848,
#27849,#27850,#27851,#27852,#27853,#27854),.UNSPECIFIED.,.F.,.F.,(4,3,3,
3,3,3,3,4),(26.2547575154336,26.873470448573,27.8687841688905,28.864097889208,
29.8594116095256,30.8547253298431,31.8500390501606,32.5379428226132),
 .UNSPECIFIED.);
#639=B_SPLINE_CURVE_WITH_KNOTS('',3,(#27859,#27860,#27861,#27862,#27863,
#27864,#27865,#27866,#27867,#27868,#27869,#27870,#27871,#27872,#27873,#27874,
#27875,#27876,#27877,#27878,#27879,#27880),.UNSPECIFIED.,.F.,.F.,(4,3,3,
3,3,3,3,4),(-41.7918608832717,-40.8078625330182,-39.8125488127007,-38.8172350923832,
-37.8219213720657,-36.8266076517482,-35.8312939314307,-35.5086755760921),
 .UNSPECIFIED.);
#640=B_SPLINE_CURVE_WITH_KNOTS('',3,(#27881,#27882,#27883,#27884,#27885,
#27886,#27887,#27888,#27889,#27890,#27891,#27892,#27893,#27894,#27895,#27896,
#27897,#27898,#27899,#27900,#27901,#27902),.UNSPECIFIED.,.F.,.F.,(4,3,3,
3,3,3,3,4),(32.5379428226132,32.8453527704781,33.8406664907956,34.8359802111131,
35.8312939314307,36.8266076517482,37.8219213720657,38.8211281297928),
 .UNSPECIFIED.);
#641=B_SPLINE_CURVE_WITH_KNOTS('',3,(#27907,#27908,#27909,#27910,#27911,
#27912,#27913,#27914,#27915,#27916,#27917,#27918,#27919,#27920,#27921,#27922,
#27923,#27924,#27925,#27926,#27927,#27928,#27929,#27930,#27931),
 .UNSPECIFIED.,.F.,.F.,(4,3,3,3,3,3,3,3,4),(-48.0750461904513,-47.7750585752409,
-46.7797448549234,-45.7844311346058,-44.7891174142883,-43.7938036939708,
-42.7984899736533,-41.8031762533358,-41.7918608832717),.UNSPECIFIED.);
#642=B_SPLINE_CURVE_WITH_KNOTS('',3,(#27932,#27933,#27934,#27935,#27936,
#27937,#27938,#27939,#27940,#27941,#27942,#27943,#27944,#27945,#27946,#27947,
#27948,#27949,#27950,#27951,#27952,#27953),.UNSPECIFIED.,.F.,.F.,(4,3,3,
3,3,3,3,4),(38.8211281297928,39.8125488127007,40.8078625330182,41.8031762533358,
42.7984899736533,43.7938036939708,44.7891174142883,45.1043134369724),
 .UNSPECIFIED.);
#643=B_SPLINE_CURVE_WITH_KNOTS('',3,(#27958,#27959,#27960,#27961,#27962,
#27963,#27964,#27965,#27966,#27967,#27968,#27969,#27970,#27971,#27972,#27973,
#27974,#27975,#27976,#27977,#27978,#27979),.UNSPECIFIED.,.F.,.F.,(4,3,3,
3,3,3,3,4),(-54.3582314976309,-53.746940897146,-52.7516271768285,-51.7563134565109,
-50.7609997361934,-49.7656860158759,-48.7703722955584,-48.0750461904513),
 .UNSPECIFIED.);
#644=B_SPLINE_CURVE_WITH_KNOTS('',3,(#27980,#27981,#27982,#27983,#27984,
#27985,#27986,#27987,#27988,#27989,#27990,#27991,#27992,#27993,#27994,#27995,
#27996,#27997,#27998,#27999,#28000,#28001),.UNSPECIFIED.,.F.,.F.,(4,3,3,
3,3,3,3,4),(45.1043134369724,45.7844311346058,46.7797448549234,47.7750585752409,
48.7703722955584,49.7656860158759,50.7609997361934,51.3874987441519),
 .UNSPECIFIED.);
#645=B_SPLINE_CURVE_WITH_KNOTS('',3,(#28006,#28007,#28008,#28009,#28010,
#28011,#28012,#28013,#28014,#28015,#28016,#28017,#28018,#28019,#28020,#28021,
#28022,#28023,#28024,#28025,#28026,#28027),.UNSPECIFIED.,.F.,.F.,(4,3,3,
3,3,3,3,4),(-60.6414168048105,-59.7188232190511,-58.7235094987336,-57.7281957784161,
-56.7328820580985,-55.737568337781,-54.7422546174635,-54.3582314976309),
 .UNSPECIFIED.);
#646=B_SPLINE_CURVE_WITH_KNOTS('',3,(#28028,#28029,#28030,#28031,#28032,
#28033,#28034,#28035,#28036,#28037,#28038,#28039,#28040,#28041,#28042,#28043,
#28044,#28045,#28046,#28047,#28048,#28049),.UNSPECIFIED.,.F.,.F.,(4,3,3,
3,3,3,3,4),(51.3874987441519,51.7563134565109,52.7516271768285,53.746940897146,
54.7422546174635,55.737568337781,56.7328820580986,57.6706840513315),
 .UNSPECIFIED.);
#647=B_SPLINE_CURVE_WITH_KNOTS('',3,(#28054,#28055,#28056,#28057,#28058,
#28059,#28060,#28061,#28062,#28063,#28064,#28065,#28066,#28067,#28068,#28069,
#28070,#28071,#28072,#28073,#28074,#28075,#28076,#28077,#28078),
 .UNSPECIFIED.,.F.,.F.,(4,3,3,3,3,3,3,3,4),(-66.9246021119901,-66.6860192612737,
-65.6907055409562,-64.6953918206387,-63.7000781003212,-62.7047643800036,
-61.7094506596861,-60.7141369393686,-60.6414168048105),.UNSPECIFIED.);
#648=B_SPLINE_CURVE_WITH_KNOTS('',3,(#28079,#28080,#28081,#28082,#28083,
#28084,#28085,#28086,#28087,#28088,#28089,#28090,#28091,#28092,#28093,#28094,
#28095,#28096,#28097,#28098,#28099,#28100,#28101,#28102,#28103),
 .UNSPECIFIED.,.F.,.F.,(4,3,3,3,3,3,3,3,4),(57.6706840513315,57.7281957784161,
58.7235094987336,59.7188232190511,60.7141369393686,61.7094506596861,62.7047643800037,
63.7000781003212,63.9538693585111),.UNSPECIFIED.);
#649=B_SPLINE_CURVE_WITH_KNOTS('',3,(#28108,#28109,#28110,#28111,#28112,
#28113,#28114,#28115,#28116,#28117,#28118,#28119,#28120,#28121,#28122,#28123,
#28124,#28125,#28126,#28127,#28128,#28129),.UNSPECIFIED.,.F.,.F.,(4,3,3,
3,3,3,3,4),(-73.2077874191697,-72.6579015831788,-71.6625878628613,-70.6672741425438,
-69.6719604222263,-68.6766467019087,-67.6813329815912,-66.9246021119901),
 .UNSPECIFIED.);
#650=B_SPLINE_CURVE_WITH_KNOTS('',3,(#28130,#28131,#28132,#28133,#28134,
#28135,#28136,#28137,#28138,#28139,#28140,#28141,#28142,#28143,#28144,#28145,
#28146,#28147,#28148,#28149,#28150,#28151),.UNSPECIFIED.,.F.,.F.,(4,3,3,
3,3,3,3,4),(63.9538693585111,64.6953918206387,65.6907055409562,66.6860192612737,
67.6813329815912,68.6766467019088,69.6719604222263,70.2370546656907),
 .UNSPECIFIED.);
#651=B_SPLINE_CURVE_WITH_KNOTS('',3,(#28156,#28157,#28158,#28159,#28160,
#28161,#28162,#28163,#28164,#28165,#28166,#28167,#28168,#28169,#28170,#28171,
#28172,#28173,#28174,#28175,#28176,#28177),.UNSPECIFIED.,.F.,.F.,(4,3,3,
3,3,3,3,4),(-79.4909727263493,-78.6297839050839,-77.6344701847664,-76.6391564644489,
-75.6438427441314,-74.6485290238139,-73.6532153034963,-73.2077874191697),
 .UNSPECIFIED.);
#652=B_SPLINE_CURVE_WITH_KNOTS('',3,(#28178,#28179,#28180,#28181,#28182,
#28183,#28184,#28185,#28186,#28187,#28188,#28189,#28190,#28191,#28192,#28193,
#28194,#28195,#28196,#28197,#28198,#28199),.UNSPECIFIED.,.F.,.F.,(4,3,3,
3,3,3,3,4),(70.2370546656907,70.6672741425438,71.6625878628613,72.6579015831788,
73.6532153034963,74.6485290238139,75.6438427441314,76.5202399728703),
 .UNSPECIFIED.);
#653=B_SPLINE_CURVE_WITH_KNOTS('',3,(#28204,#28205,#28206,#28207,#28208,
#28209,#28210,#28211,#28212,#28213,#28214,#28215,#28216,#28217,#28218,#28219,
#28220,#28221,#28222,#28223,#28224,#28225,#28226,#28227,#28228),
 .UNSPECIFIED.,.F.,.F.,(4,3,3,3,3,3,3,3,4),(-85.7741580335289,-85.5969799473066,
-84.601666226989,-83.6063525066715,-82.611038786354,-81.6157250660365,-80.620411345719,
-79.6250976254015,-79.4909727263493),.UNSPECIFIED.);
#654=B_SPLINE_CURVE_WITH_KNOTS('',3,(#28229,#28230,#28231,#28232,#28233,
#28234,#28235,#28236,#28237,#28238,#28239,#28240,#28241,#28242,#28243,#28244,
#28245,#28246,#28247,#28248,#28249,#28250,#28251,#28252,#28253),
 .UNSPECIFIED.,.F.,.F.,(4,3,3,3,3,3,3,3,4),(76.5202399728703,76.6391564644489,
77.6344701847664,78.6297839050839,79.6250976254015,80.620411345719,81.6157250660365,
82.611038786354,82.8034252800499),.UNSPECIFIED.);
#655=B_SPLINE_CURVE_WITH_KNOTS('',3,(#28258,#28259,#28260,#28261,#28262,
#28263,#28264,#28265,#28266,#28267,#28268,#28269,#28270,#28271,#28272,#28273,
#28274,#28275,#28276,#28277,#28278,#28279),.UNSPECIFIED.,.F.,.F.,(4,3,3,
3,3,3,3,4),(-92.0573433407085,-91.5688622692116,-90.5735485488942,-89.5782348285766,
-88.5829211082591,-87.5876073879416,-86.5922936676241,-85.7741580335289),
 .UNSPECIFIED.);
#656=B_SPLINE_CURVE_WITH_KNOTS('',3,(#28280,#28281,#28282,#28283,#28284,
#28285,#28286,#28287,#28288,#28289,#28290,#28291,#28292,#28293,#28294,#28295,
#28296,#28297,#28298,#28299,#28300,#28301),.UNSPECIFIED.,.F.,.F.,(4,3,3,
3,3,3,3,4),(82.8034252800499,83.6063525066715,84.6016662269891,85.5969799473066,
86.5922936676241,87.5876073879416,88.5829211082591,89.0866105872295),
 .UNSPECIFIED.);
#657=B_SPLINE_CURVE_WITH_KNOTS('',3,(#28306,#28307,#28308,#28309,#28310,
#28311,#28312,#28313,#28314,#28315,#28316,#28317,#28318,#28319,#28320,#28321,
#28322,#28323,#28324,#28325,#28326,#28327),.UNSPECIFIED.,.F.,.F.,(4,3,3,
3,3,3,3,4),(-98.3405286478881,-97.5407445911168,-96.5454308707993,-95.5501171504817,
-94.5548034301642,-93.5594897098467,-92.5641759895292,-92.0573433407085),
 .UNSPECIFIED.);
#658=B_SPLINE_CURVE_WITH_KNOTS('',3,(#28328,#28329,#28330,#28331,#28332,
#28333,#28334,#28335,#28336,#28337,#28338,#28339,#28340,#28341,#28342,#28343,
#28344,#28345,#28346,#28347,#28348,#28349),.UNSPECIFIED.,.F.,.F.,(4,3,3,
3,3,3,3,4),(89.0866105872295,89.5782348285766,90.5735485488942,91.5688622692117,
92.5641759895292,93.5594897098467,94.5548034301642,95.3697958944091),
 .UNSPECIFIED.);
#659=B_SPLINE_CURVE_WITH_KNOTS('',3,(#28354,#28355,#28356,#28357,#28358,
#28359,#28360,#28361,#28362,#28363,#28364,#28365,#28366,#28367,#28368,#28369,
#28370,#28371,#28372,#28373,#28374,#28375,#28376,#28377,#28378),
 .UNSPECIFIED.,.F.,.F.,(4,3,3,3,3,3,3,3,4),(-104.623713955068,-104.507940633339,
-103.512626913022,-102.517313192704,-101.521999472387,-100.526685752069,
-99.5313720317518,-98.5360583114343,-98.3405286478881),.UNSPECIFIED.);
#660=B_SPLINE_CURVE_WITH_KNOTS('',3,(#28379,#28380,#28381,#28382,#28383,
#28384,#28385,#28386,#28387,#28388,#28389,#28390,#28391,#28392,#28393,#28394,
#28395,#28396,#28397,#28398,#28399,#28400,#28401,#28402,#28403),
 .UNSPECIFIED.,.F.,.F.,(4,3,3,3,3,3,3,3,4),(95.3697958944091,95.5501171504818,
96.5454308707993,97.5407445911168,98.5360583114343,99.5313720317518,100.526685752069,
101.521999472387,101.652981201589),.UNSPECIFIED.);
#661=B_SPLINE_CURVE_WITH_KNOTS('',3,(#28408,#28409,#28410,#28411,#28412,
#28413,#28414,#28415,#28416,#28417,#28418,#28419,#28420,#28421,#28422,#28423,
#28424,#28425,#28426,#28427,#28428,#28429),.UNSPECIFIED.,.F.,.F.,(4,3,3,
3,3,3,3,4),(-110.906899262247,-110.479822955245,-109.484509234927,-108.489195514609,
-107.493881794292,-106.498568073974,-105.503254353657,-104.623713955068),
 .UNSPECIFIED.);
#662=B_SPLINE_CURVE_WITH_KNOTS('',3,(#28430,#28431,#28432,#28433,#28434,
#28435,#28436,#28437,#28438,#28439,#28440,#28441,#28442,#28443,#28444,#28445,
#28446,#28447,#28448,#28449,#28450,#28451),.UNSPECIFIED.,.F.,.F.,(4,3,3,
3,3,3,3,4),(101.652981201589,102.517313192704,103.512626913022,104.507940633339,
105.503254353657,106.498568073974,107.493881794292,107.936166508768),
 .UNSPECIFIED.);
#663=B_SPLINE_CURVE_WITH_KNOTS('',3,(#28456,#28457,#28458,#28459,#28460,
#28461,#28462,#28463,#28464,#28465,#28466,#28467,#28468,#28469,#28470,#28471,
#28472,#28473,#28474,#28475,#28476,#28477),.UNSPECIFIED.,.F.,.F.,(4,3,3,
3,3,3,3,4),(-117.190084569427,-116.45170527715,-115.456391556832,-114.461077836515,
-113.465764116197,-112.47045039588,-111.475136675562,-110.906899262247),
 .UNSPECIFIED.);
#664=B_SPLINE_CURVE_WITH_KNOTS('',3,(#28478,#28479,#28480,#28481,#28482,
#28483,#28484,#28485,#28486,#28487,#28488,#28489,#28490,#28491,#28492,#28493,
#28494,#28495,#28496,#28497,#28498,#28499),.UNSPECIFIED.,.F.,.F.,(4,3,3,
3,3,3,3,4),(107.936166508768,108.48919551461,109.484509234927,110.479822955245,
111.475136675562,112.47045039588,113.465764116197,114.219351815948),
 .UNSPECIFIED.);
#665=B_SPLINE_CURVE_WITH_KNOTS('',3,(#28504,#28505,#28506,#28507,#28508,
#28509,#28510,#28511,#28512,#28513,#28514,#28515,#28516,#28517,#28518,#28519,
#28520,#28521,#28522,#28523,#28524,#28525,#28526,#28527,#28528),
 .UNSPECIFIED.,.F.,.F.,(4,3,3,3,3,3,3,3,4),(-123.473269876606,-123.418901319372,
-122.423587599055,-121.428273878737,-120.43296015842,-119.437646438102,
-118.442332717785,-117.447018997467,-117.190084569427),.UNSPECIFIED.);
#666=B_SPLINE_CURVE_WITH_KNOTS('',3,(#28529,#28530,#28531,#28532,#28533,
#28534,#28535,#28536,#28537,#28538,#28539,#28540,#28541,#28542,#28543,#28544,
#28545,#28546,#28547,#28548,#28549,#28550,#28551,#28552,#28553),
 .UNSPECIFIED.,.F.,.F.,(4,3,3,3,3,3,3,3,4),(114.219351815948,114.461077836515,
115.456391556832,116.45170527715,117.447018997467,118.442332717785,119.437646438102,
120.43296015842,120.502537123127),.UNSPECIFIED.);
#667=B_SPLINE_CURVE_WITH_KNOTS('',3,(#28558,#28559,#28560,#28561,#28562,
#28563,#28564,#28565,#28566,#28567,#28568,#28569,#28570,#28571,#28572,#28573,
#28574,#28575,#28576,#28577,#28578,#28579),.UNSPECIFIED.,.F.,.F.,(4,3,3,
3,3,3,3,4),(-129.756455183786,-129.390783641277,-128.39546992096,-127.400156200642,
-126.404842480325,-125.409528760007,-124.41421503969,-123.473269876606),
 .UNSPECIFIED.);
#668=B_SPLINE_CURVE_WITH_KNOTS('',3,(#28580,#28581,#28582,#28583,#28584,
#28585,#28586,#28587,#28588,#28589,#28590,#28591,#28592,#28593,#28594,#28595,
#28596,#28597,#28598,#28599,#28600,#28601),.UNSPECIFIED.,.F.,.F.,(4,3,3,
3,3,3,3,4),(120.502537123127,121.428273878737,122.423587599055,123.418901319372,
124.41421503969,125.409528760007,126.404842480325,126.785722430307),
 .UNSPECIFIED.);
#669=B_SPLINE_CURVE_WITH_KNOTS('',3,(#28606,#28607,#28608,#28609,#28610,
#28611,#28612,#28613,#28614,#28615,#28616,#28617,#28618,#28619,#28620,#28621,
#28622,#28623,#28624,#28625,#28626,#28627),.UNSPECIFIED.,.F.,.F.,(4,3,3,
3,3,3,3,4),(-136.039640490966,-135.362665963182,-134.367352242865,-133.372038522547,
-132.37672480223,-131.381411081912,-130.386097361595,-129.756455183786),
 .UNSPECIFIED.);
#670=B_SPLINE_CURVE_WITH_KNOTS('',3,(#28628,#28629,#28630,#28631,#28632,
#28633,#28634,#28635,#28636,#28637,#28638,#28639,#28640,#28641,#28642,#28643,
#28644,#28645,#28646,#28647,#28648,#28649),.UNSPECIFIED.,.F.,.F.,(4,3,3,
3,3,3,3,4),(126.785722430307,127.400156200642,128.39546992096,129.390783641277,
130.386097361595,131.381411081912,132.37672480223,133.068907737487),
 .UNSPECIFIED.);
#671=B_SPLINE_CURVE_WITH_KNOTS('',3,(#28654,#28655,#28656,#28657,#28658,
#28659,#28660,#28661,#28662,#28663,#28664,#28665,#28666,#28667,#28668,#28669,
#28670,#28671,#28672,#28673,#28674,#28675),.UNSPECIFIED.,.F.,.F.,(4,3,3,
3,3,3,3,4),(-142.322825798145,-141.334548285088,-140.33923456477,-139.343920844453,
-138.348607124135,-137.353293403818,-136.3579796835,-136.039640490966),
 .UNSPECIFIED.);
#672=B_SPLINE_CURVE_WITH_KNOTS('',3,(#28676,#28677,#28678,#28679,#28680,
#28681,#28682,#28683,#28684,#28685,#28686,#28687,#28688,#28689,#28690,#28691,
#28692,#28693,#28694,#28695,#28696,#28697,#28698,#28699,#28700),
 .UNSPECIFIED.,.F.,.F.,(4,3,3,3,3,3,3,3,4),(133.068907737487,133.372038522547,
134.367352242865,135.362665963182,136.3579796835,137.353293403818,138.348607124135,
139.343920844453,139.352093044666),.UNSPECIFIED.);
#673=B_SPLINE_CURVE_WITH_KNOTS('',3,(#28707,#28708,#28709,#28710,#28711,
#28712,#28713,#28714,#28715,#28716,#28717,#28718,#28719,#28720,#28721,#28722,
#28723,#28724,#28725,#28726,#28727,#28728),.UNSPECIFIED.,.F.,.F.,(4,3,3,
3,3,3,3,4),(-148.30174432731,-147.306430606993,-146.311116886675,-145.315803166358,
-144.32048944604,-143.325175725723,-142.329862005405,-142.322825798145),
 .UNSPECIFIED.);
#674=B_SPLINE_CURVE_WITH_KNOTS('',3,(#28729,#28730,#28731,#28732,#28733,
#28734,#28735,#28736,#28737,#28738,#28739,#28740,#28741,#28742,#28743,#28744,
#28745,#28746,#28747,#28748,#28749,#28750),.UNSPECIFIED.,.F.,.F.,(4,3,3,
3,3,3,3,4),(139.352093044666,140.33923456477,141.334548285088,142.329862005405,
143.325175725723,144.32048944604,145.315803166358,145.635278351846),
 .UNSPECIFIED.);
#675=B_SPLINE_CURVE_WITH_KNOTS('',3,(#28756,#28757,#28758,#28759,#28760,
#28761,#28762,#28763),.UNSPECIFIED.,.F.,.F.,(4,1,1,1,1,4),(153.9380400259,
153.94507623316,154.940389953477,155.935703673795,156.931017394112,157.843785881745),
 .UNSPECIFIED.);
#676=B_SPLINE_CURVE_WITH_KNOTS('',3,(#28766,#28767,#28768,#28769,#28770,
#28771),.UNSPECIFIED.,.F.,.F.,(4,1,1,4),(153.9380400259,154.613878560729,
155.609192281047,156.604506001364),.UNSPECIFIED.);
#677=B_SPLINE_CURVE_WITH_KNOTS('',3,(#28776,#28777,#28778,#28779,#28780,
#28781,#28782,#28783,#28784,#28785),.UNSPECIFIED.,.F.,.F.,(4,1,1,1,1,1,
1,4),(147.65485471872,147.973193911255,148.968507631572,149.96382135189,
150.959135072207,151.954448792525,152.949762512842,153.9380400259),
 .UNSPECIFIED.);
#678=B_SPLINE_CURVE_WITH_KNOTS('',3,(#28786,#28787,#28788,#28789,#28790,
#28791,#28792,#28793,#28794,#28795),.UNSPECIFIED.,.F.,.F.,(4,1,1,1,1,1,
1,4),(147.65485471872,148.641996238824,149.637309959142,150.632623679459,
151.627937399777,152.623251120094,153.618564840412,153.9380400259),
 .UNSPECIFIED.);
#679=B_SPLINE_CURVE_WITH_KNOTS('',3,(#28800,#28801,#28802,#28803,#28804,
#28805,#28806,#28807,#28808,#28809),.UNSPECIFIED.,.F.,.F.,(4,1,1,1,1,1,
1,4),(141.371669411541,142.00131158935,142.996625309667,143.991939029985,
144.987252750302,145.98256647062,146.977880190937,147.65485471872),
 .UNSPECIFIED.);
#680=B_SPLINE_CURVE_WITH_KNOTS('',3,(#28810,#28811,#28812,#28813,#28814,
#28815,#28816,#28817,#28818,#28819,#28820),.UNSPECIFIED.,.F.,.F.,(4,1,1,
1,1,1,1,1,4),(141.371669411541,141.674800196602,142.670113916919,143.665427637237,
144.660741357554,145.656055077872,146.651368798189,147.646682518507,147.65485471872),
 .UNSPECIFIED.);
#681=B_SPLINE_CURVE_WITH_KNOTS('',3,(#28825,#28826,#28827,#28828,#28829,
#28830,#28831,#28832,#28833,#28834),.UNSPECIFIED.,.F.,.F.,(4,1,1,1,1,1,
1,4),(135.088484104361,136.029429267445,137.024742987762,138.02005670808,
139.015370428397,140.010684148715,141.005997869032,141.371669411541),
 .UNSPECIFIED.);
#682=B_SPLINE_CURVE_WITH_KNOTS('',3,(#28835,#28836,#28837,#28838,#28839,
#28840,#28841,#28842,#28843,#28844),.UNSPECIFIED.,.F.,.F.,(4,1,1,1,1,1,
1,4),(135.088484104361,135.702917874696,136.698231595014,137.693545315331,
138.688859035649,139.684172755966,140.679486476284,141.371669411541),
 .UNSPECIFIED.);
#683=B_SPLINE_CURVE_WITH_KNOTS('',3,(#28849,#28850,#28851,#28852,#28853,
#28854,#28855,#28856,#28857,#28858,#28859),.UNSPECIFIED.,.F.,.F.,(4,1,1,
1,1,1,1,1,4),(128.805298797182,129.062233225222,130.057546945539,131.052860665857,
132.048174386174,133.043488106492,134.038801826809,135.034115547127,135.088484104361),
 .UNSPECIFIED.);
#684=B_SPLINE_CURVE_WITH_KNOTS('',3,(#28860,#28861,#28862,#28863,#28864,
#28865,#28866,#28867,#28868,#28869),.UNSPECIFIED.,.F.,.F.,(4,1,1,1,1,1,
1,4),(128.805298797182,129.731035552791,130.726349273109,131.721662993426,
132.716976713744,133.712290434061,134.707604154379,135.088484104361),
 .UNSPECIFIED.);
#685=B_SPLINE_CURVE_WITH_KNOTS('',3,(#28874,#28875,#28876,#28877,#28878,
#28879,#28880,#28881,#28882,#28883),.UNSPECIFIED.,.F.,.F.,(4,1,1,1,1,1,
1,4),(122.522113490002,123.090350903317,124.085664623634,125.080978343952,
126.076292064269,127.071605784587,128.066919504904,128.805298797182),
 .UNSPECIFIED.);
#686=B_SPLINE_CURVE_WITH_KNOTS('',3,(#28884,#28885,#28886,#28887,#28888,
#28889,#28890,#28891,#28892,#28893,#28894),.UNSPECIFIED.,.F.,.F.,(4,1,1,
1,1,1,1,1,4),(122.522113490002,122.763839510569,123.759153230886,124.754466951204,
125.749780671521,126.745094391839,127.740408112156,128.735721832474,128.805298797182),
 .UNSPECIFIED.);
#687=B_SPLINE_CURVE_WITH_KNOTS('',3,(#28899,#28900,#28901,#28902,#28903,
#28904,#28905,#28906,#28907,#28908),.UNSPECIFIED.,.F.,.F.,(4,1,1,1,1,1,
1,4),(116.238928182822,117.118468581412,118.113782301729,119.109096022047,
120.104409742364,121.099723462682,122.095037182999,122.522113490002),
 .UNSPECIFIED.);
#688=B_SPLINE_CURVE_WITH_KNOTS('',3,(#28909,#28910,#28911,#28912,#28913,
#28914,#28915,#28916,#28917,#28918),.UNSPECIFIED.,.F.,.F.,(4,1,1,1,1,1,
1,4),(116.238928182822,116.791957188664,117.787270908981,118.782584629299,
119.777898349616,120.773212069934,121.768525790251,122.522113490002),
 .UNSPECIFIED.);
#689=B_SPLINE_CURVE_WITH_KNOTS('',3,(#28923,#28924,#28925,#28926,#28927,
#28928,#28929,#28930,#28931,#28932,#28933),.UNSPECIFIED.,.F.,.F.,(4,1,1,
1,1,1,1,1,4),(109.955742875643,110.151272539189,111.146586259507,112.141899979824,
113.137213700142,114.132527420459,115.127841140777,116.123154861094,116.238928182822),
 .UNSPECIFIED.);
#690=B_SPLINE_CURVE_WITH_KNOTS('',3,(#28934,#28935,#28936,#28937,#28938,
#28939,#28940,#28941,#28942,#28943),.UNSPECIFIED.,.F.,.F.,(4,1,1,1,1,1,
1,4),(109.955742875643,110.820074866758,111.815388587076,112.810702307393,
113.806016027711,114.801329748029,115.796643468346,116.238928182822),
 .UNSPECIFIED.);
#691=B_SPLINE_CURVE_WITH_KNOTS('',3,(#28948,#28949,#28950,#28951,#28952,
#28953,#28954,#28955,#28956,#28957),.UNSPECIFIED.,.F.,.F.,(4,1,1,1,1,1,
1,4),(103.672557568463,104.179390217284,105.174703937601,106.170017657919,
107.165331378236,108.160645098554,109.155958818872,109.955742875643),
 .UNSPECIFIED.);
#692=B_SPLINE_CURVE_WITH_KNOTS('',3,(#28958,#28959,#28960,#28961,#28962,
#28963,#28964,#28965,#28966,#28967,#28968),.UNSPECIFIED.,.F.,.F.,(4,1,1,
1,1,1,1,1,4),(103.672557568463,103.852878824536,104.848192544853,105.843506265171,
106.838819985488,107.834133705806,108.829447426123,109.824761146441,109.955742875643),
 .UNSPECIFIED.);
#693=B_SPLINE_CURVE_WITH_KNOTS('',3,(#28973,#28974,#28975,#28976,#28977,
#28978,#28979,#28980,#28981,#28982),.UNSPECIFIED.,.F.,.F.,(4,1,1,1,1,1,
1,4),(97.3893722612837,98.2075078953788,99.2028216156963,100.198135336014,
101.193449056331,102.188762776649,103.184076496966,103.672557568463),
 .UNSPECIFIED.);
#694=B_SPLINE_CURVE_WITH_KNOTS('',3,(#28983,#28984,#28985,#28986,#28987,
#28988,#28989,#28990,#28991,#28992),.UNSPECIFIED.,.F.,.F.,(4,1,1,1,1,1,
1,4),(97.3893722612836,97.8809965026307,98.8763102229482,99.8716239432658,
100.866937663583,101.862251383901,102.857565104218,103.672557568463),
 .UNSPECIFIED.);
#695=B_SPLINE_CURVE_WITH_KNOTS('',3,(#28997,#28998,#28999,#29000,#29001,
#29002,#29003,#29004,#29005,#29006,#29007),.UNSPECIFIED.,.F.,.F.,(4,1,1,
1,1,1,1,1,4),(91.106186954104,91.2403118531562,92.2356255734737,93.2309392937912,
94.2262530141087,95.2215667344263,96.2168804547438,97.2121941750613,97.3893722612837),
 .UNSPECIFIED.);
#696=B_SPLINE_CURVE_WITH_KNOTS('',3,(#29008,#29009,#29010,#29011,#29012,
#29013,#29014,#29015,#29016,#29017),.UNSPECIFIED.,.F.,.F.,(4,1,1,1,1,1,
1,4),(91.106186954104,91.9091141807256,92.9044279010431,93.8997416213606,
94.8950553416782,95.8903690619957,96.8856827823132,97.3893722612836),
 .UNSPECIFIED.);
#697=B_SPLINE_CURVE_WITH_KNOTS('',3,(#29022,#29023,#29024,#29025,#29026,
#29027,#29028,#29029,#29030,#29031),.UNSPECIFIED.,.F.,.F.,(4,1,1,1,1,1,
1,4),(84.8230016469244,85.2684295312511,86.2637432515686,87.2590569718861,
88.2543706922037,89.2496844125212,90.2449981328387,91.106186954104),
 .UNSPECIFIED.);
#698=B_SPLINE_CURVE_WITH_KNOTS('',3,(#29032,#29033,#29034,#29035,#29036,
#29037,#29038,#29039,#29040,#29041,#29042),.UNSPECIFIED.,.F.,.F.,(4,1,1,
1,1,1,1,1,4),(84.8230016469244,84.941918138503,85.9372318588205,86.932545579138,
87.9278592994555,88.9231730197731,89.9184867400906,90.9138004604081,91.106186954104),
 .UNSPECIFIED.);
#699=B_SPLINE_CURVE_WITH_KNOTS('',3,(#29047,#29048,#29049,#29050,#29051,
#29052,#29053,#29054,#29055,#29056),.UNSPECIFIED.,.F.,.F.,(4,1,1,1,1,1,
1,4),(78.5398163397449,79.296547209346,80.2918609296635,81.287174649981,
82.2824883702986,83.2778020906161,84.2731158109336,84.8230016469244),
 .UNSPECIFIED.);
#700=B_SPLINE_CURVE_WITH_KNOTS('',3,(#29057,#29058,#29059,#29060,#29061,
#29062,#29063,#29064,#29065,#29066),.UNSPECIFIED.,.F.,.F.,(4,1,1,1,1,1,
1,4),(78.5398163397448,78.9700358165979,79.9653495369154,80.9606632572329,
81.9559769775504,82.9512906978679,83.9466044181855,84.8230016469244),
 .UNSPECIFIED.);
#701=B_SPLINE_CURVE_WITH_KNOTS('',3,(#29071,#29072,#29073,#29074,#29075,
#29076,#29077,#29078,#29079,#29080,#29081),.UNSPECIFIED.,.F.,.F.,(4,1,1,
1,1,1,1,1,4),(72.2566310325653,72.3293511671233,73.3246648874409,74.3199786077584,
75.3152923280759,76.3106060483934,77.3059197687109,78.3012334890285,78.5398163397449),
 .UNSPECIFIED.);
#702=B_SPLINE_CURVE_WITH_KNOTS('',3,(#29082,#29083,#29084,#29085,#29086,
#29087,#29088,#29089,#29090,#29091),.UNSPECIFIED.,.F.,.F.,(4,1,1,1,1,1,
1,4),(72.2566310325653,72.9981534946928,73.9934672150103,74.9887809353278,
75.9840946556453,76.9794083759628,77.9747220962804,78.5398163397448),
 .UNSPECIFIED.);
#703=B_SPLINE_CURVE_WITH_KNOTS('',3,(#29096,#29097,#29098,#29099,#29100,
#29101,#29102,#29103,#29104,#29105),.UNSPECIFIED.,.F.,.F.,(4,1,1,1,1,1,
1,4),(65.9734457253857,66.3574688452182,67.3527825655358,68.3480962858533,
69.3434100061708,70.3387237264883,71.3340374468058,72.2566310325653),
 .UNSPECIFIED.);
#704=B_SPLINE_CURVE_WITH_KNOTS('',3,(#29106,#29107,#29108,#29109,#29110,
#29111,#29112,#29113,#29114,#29115,#29116),.UNSPECIFIED.,.F.,.F.,(4,1,1,
1,1,1,1,1,4),(65.9734457253856,66.0309574524701,67.0262711727877,68.0215848931052,
69.0168986134227,70.0122123337402,71.0075260540577,72.0028397743752,72.2566310325653),
 .UNSPECIFIED.);
#705=B_SPLINE_CURVE_WITH_KNOTS('',3,(#29121,#29122,#29123,#29124,#29125,
#29126,#29127,#29128,#29129,#29130),.UNSPECIFIED.,.F.,.F.,(4,1,1,1,1,1,
1,4),(59.6902604182061,60.3855865233131,61.3809002436307,62.3762139639482,
63.3715276842657,64.3668414045832,65.3621551249007,65.9734457253857),
 .UNSPECIFIED.);
#706=B_SPLINE_CURVE_WITH_KNOTS('',3,(#29131,#29132,#29133,#29134,#29135,
#29136,#29137,#29138,#29139,#29140),.UNSPECIFIED.,.F.,.F.,(4,1,1,1,1,1,
1,4),(59.6902604182061,60.059075130565,61.0543888508825,62.0497025712001,
63.0450162915176,64.0403300118351,65.0356437321526,65.9734457253856),
 .UNSPECIFIED.);
#707=B_SPLINE_CURVE_WITH_KNOTS('',3,(#29145,#29146,#29147,#29148,#29149,
#29150,#29151,#29152,#29153,#29154,#29155),.UNSPECIFIED.,.F.,.F.,(4,1,1,
1,1,1,1,1,4),(53.4070751110265,53.4183904810905,54.413704201408,55.4090179217255,
56.4043316420431,57.3996453623606,58.3949590826781,59.3902728029956,59.6902604182061),
 .UNSPECIFIED.);
#708=B_SPLINE_CURVE_WITH_KNOTS('',3,(#29156,#29157,#29158,#29159,#29160,
#29161,#29162,#29163,#29164,#29165),.UNSPECIFIED.,.F.,.F.,(4,1,1,1,1,1,
1,4),(53.4070751110265,54.0871928086599,55.0825065289774,56.077820249295,
57.0731339696125,58.06844768993,59.0637614102475,59.6902604182061),
 .UNSPECIFIED.);
#709=B_SPLINE_CURVE_WITH_KNOTS('',3,(#29170,#29171,#29172,#29173,#29174,
#29175,#29176,#29177,#29178,#29179),.UNSPECIFIED.,.F.,.F.,(4,1,1,1,1,1,
1,4),(47.1238898038469,47.4465081591854,48.4418218795029,49.4371355998204,
50.432449320138,51.4277630404555,52.423076760773,53.4070751110265),
 .UNSPECIFIED.);
#710=B_SPLINE_CURVE_WITH_KNOTS('',3,(#29180,#29181,#29182,#29183,#29184,
#29185,#29186,#29187,#29188,#29189),.UNSPECIFIED.,.F.,.F.,(4,1,1,1,1,1,
1,4),(47.1238898038469,48.1153104867548,49.1106242070723,50.1059379273898,
51.1012516477074,52.0965653680249,53.0918790883424,53.4070751110265),
 .UNSPECIFIED.);
#711=B_SPLINE_CURVE_WITH_KNOTS('',3,(#29194,#29195,#29196,#29197,#29198,
#29199,#29200,#29201,#29202,#29203),.UNSPECIFIED.,.F.,.F.,(4,1,1,1,1,1,
1,4),(40.8407044966673,41.4746258372803,42.4699395575978,43.4652532779153,
44.4605669982328,45.4558807185504,46.4511944388679,47.1238898038469),
 .UNSPECIFIED.);
#712=B_SPLINE_CURVE_WITH_KNOTS('',3,(#29204,#29205,#29206,#29207,#29208,
#29209,#29210,#29211,#29212,#29213,#29214),.UNSPECIFIED.,.F.,.F.,(4,1,1,
1,1,1,1,1,4),(40.8407044966673,41.1481144445322,42.1434281648497,43.1387418851672,
44.1340556054847,45.1293693258023,46.1246830461198,47.1199967664373,47.1238898038469),
 .UNSPECIFIED.);
#713=B_SPLINE_CURVE_WITH_KNOTS('',3,(#29219,#29220,#29221,#29222,#29223,
#29224,#29225,#29226,#29227,#29228),.UNSPECIFIED.,.F.,.F.,(4,1,1,1,1,1,
1,4),(34.5575191894877,35.5027435153752,36.4980572356927,37.4933709560102,
38.4886846763277,39.4839983966453,40.4793121169628,40.8407044966673),
 .UNSPECIFIED.);
#714=B_SPLINE_CURVE_WITH_KNOTS('',3,(#29229,#29230,#29231,#29232,#29233,
#29234,#29235,#29236,#29237,#29238),.UNSPECIFIED.,.F.,.F.,(4,1,1,1,1,1,
1,4),(34.5575191894877,35.1762321226271,36.1715458429446,37.1668595632621,
38.1621732835796,39.1574870038972,40.1528007242147,40.8407044966673),
 .UNSPECIFIED.);
#715=B_SPLINE_CURVE_WITH_KNOTS('',3,(#29243,#29244,#29245,#29246,#29247,
#29248,#29249,#29250,#29251,#29252,#29253),.UNSPECIFIED.,.F.,.F.,(4,1,1,
1,1,1,1,1,4),(28.2743338823081,28.5355474731526,29.5308611934701,30.5261749137876,
31.5214886341051,32.5168023544226,33.5121160747401,34.5074297950577,34.5575191894877),
 .UNSPECIFIED.);
#716=B_SPLINE_CURVE_WITH_KNOTS('',3,(#29254,#29255,#29256,#29257,#29258,
#29259,#29260,#29261,#29262,#29263),.UNSPECIFIED.,.F.,.F.,(4,1,1,1,1,1,
1,4),(28.2743338823081,29.204349800722,30.1996635210395,31.194977241357,
32.1902909616745,33.185604681992,34.1809184023096,34.5575191894877),
 .UNSPECIFIED.);
#717=B_SPLINE_CURVE_WITH_KNOTS('',3,(#29268,#29269,#29270,#29271,#29272,
#29273,#29274,#29275,#29276,#29277),.UNSPECIFIED.,.F.,.F.,(4,1,1,1,1,1,
1,4),(21.9911485751286,22.5636651512475,23.558978871565,24.5542925918825,
25.5496063122,26.5449200325175,27.540233752835,28.2743338823081),
 .UNSPECIFIED.);
#718=B_SPLINE_CURVE_WITH_KNOTS('',3,(#29278,#29279,#29280,#29281,#29282,
#29283,#29284,#29285,#29286,#29287,#29288),.UNSPECIFIED.,.F.,.F.,(4,1,1,
1,1,1,1,1,4),(21.9911485751285,22.2371537584993,23.2324674788169,24.2277811991344,
25.2230949194519,26.2184086397694,27.2137223600869,28.2090360804045,28.2743338823081),
 .UNSPECIFIED.);
#719=B_SPLINE_CURVE_WITH_KNOTS('',3,(#29293,#29294,#29295,#29296,#29297,
#29298,#29299,#29300,#29301,#29302),.UNSPECIFIED.,.F.,.F.,(4,1,1,1,1,1,
1,4),(15.707963267949,16.5917828293423,17.5870965496599,18.5824102699774,
19.5777239902949,20.5730377106124,21.5683514309299,21.9911485751286),
 .UNSPECIFIED.);
#720=B_SPLINE_CURVE_WITH_KNOTS('',3,(#29303,#29304,#29305,#29306,#29307,
#29308,#29309,#29310,#29311,#29312),.UNSPECIFIED.,.F.,.F.,(4,1,1,1,1,1,
1,4),(15.7079632679489,16.2652714365942,17.2605851569118,18.2558988772293,
19.2512125975468,20.2465263178643,21.2418400381818,21.9911485751285),
 .UNSPECIFIED.);
#721=B_SPLINE_CURVE_WITH_KNOTS('',3,(#29954,#29955,#29956,#29957,#29958,
#29959,#29960,#29961,#29962,#29963,#29964,#29965,#29966,#29967,#29968,#29969,
#29970,#29971,#29972,#29973,#29974,#29975,#29976,#29977,#29978,#29979,#29980,
#29981,#29982,#29983,#29984,#29985,#29986,#29987,#29988,#29989,#29990,#29991,
#29992,#29993,#29994,#29995,#29996,#29997,#29998,#29999,#30000,#30001,#30002,
#30003,#30004,#30005,#30006,#30007,#30008),.UNSPECIFIED.,.F.,.F.,(4,3,3,
3,3,3,3,3,3,3,3,3,3,3,3,3,3,3,4),(-0.482632075205622,-0.462336249281047,
-0.427687003019698,-0.408173644600383,-0.380690085942371,-0.361844801684832,
-0.34704441187773,-0.301818556126274,-0.266377775059192,-0.255314335513618,
-0.224577305012635,-0.190497645767355,-0.176369177709915,-0.165433267624407,
-0.124074950718305,-0.0869433870803508,-0.0742996259130463,-0.032357512502151,
0.),.UNSPECIFIED.);
#722=B_SPLINE_CURVE_WITH_KNOTS('',3,(#30009,#30010,#30011,#30012),
 .UNSPECIFIED.,.F.,.F.,(4,4),(145.635278351846,146.22857165399),
 .UNSPECIFIED.);
#723=B_SPLINE_CURVE_WITH_KNOTS('',3,(#30014,#30015,#30016,#30017,#30018,
#30019,#30020,#30021,#30022,#30023,#30024,#30025,#30026,#30027,#30028,#30029,
#30030,#30031,#30032,#30033,#30034,#30035,#30036,#30037,#30038,#30039,#30040,
#30041,#30042,#30043,#30044,#30045,#30046,#30047,#30048,#30049,#30050,#30051,
#30052,#30053,#30054,#30055,#30056,#30057,#30058,#30059,#30060,#30061,#30062,
#30063,#30064,#30065,#30066,#30067,#30068),.UNSPECIFIED.,.F.,.F.,(4,3,3,
3,3,3,3,3,3,3,3,3,3,3,3,3,3,3,4),(-0.483882268593951,-0.46576353335263,
-0.430852383331094,-0.416229815277715,-0.375093755185218,-0.358591999734009,
-0.314305848550002,-0.283376081257857,-0.270874225938811,-0.239681235538259,
-0.209721081095977,-0.193164961501836,-0.179875924261507,-0.13490694319613,
-0.112773483820775,-0.0967277303364094,-0.0829938450850564,-0.0368476966362759,
0.),.UNSPECIFIED.);
#724=B_SPLINE_CURVE_WITH_KNOTS('',3,(#30069,#30070,#30071,#30072,#30073,
#30074,#30075,#30076,#30077),.UNSPECIFIED.,.F.,.F.,(4,1,1,1,1,1,4),(10.3759343473738,
11.2887028350066,12.2840165553242,13.2793302756417,14.2746439959592,15.2699577162767,
15.7079632679489),.UNSPECIFIED.);
#725=B_SPLINE_CURVE_WITH_KNOTS('',3,(#30083,#30084,#30085,#30086,#30087,
#30088,#30089,#30090,#30091,#30092,#30093,#30094,#30095,#30096,#30097,#30098,
#30099,#30100,#30101,#30102,#30103,#30104,#30105,#30106,#30107,#30108,#30109,
#30110,#30111,#30112,#30113,#30114,#30115,#30116,#30117,#30118,#30119,#30120,
#30121,#30122,#30123,#30124,#30125,#30126,#30127,#30128,#30129,#30130,#30131,
#30132,#30133,#30134,#30135,#30136,#30137),.UNSPECIFIED.,.F.,.F.,(4,3,3,
3,3,3,3,3,3,3,3,3,3,3,3,3,3,3,4),(-0.482632075205632,-0.462336249281051,
-0.427686999954685,-0.408173642759644,-0.380690078686806,-0.361844802480269,
-0.347044410218777,-0.301818552387021,-0.26637777077025,-0.255314327560454,
-0.224577305012648,-0.190497642723496,-0.176369168534599,-0.16543325457945,
-0.124074940934588,-0.0869433711633969,-0.0742996240346052,-0.0323575236186803,
0.),.UNSPECIFIED.);
#726=B_SPLINE_CURVE_WITH_KNOTS('',3,(#30140,#30141,#30142,#30143,#30144,
#30145,#30146,#30147),.UNSPECIFIED.,.F.,.F.,(4,1,1,1,1,4),(11.6152142277548,
12.6105279480723,13.6058416683898,14.6011553887073,15.5964691090248,15.707963267949),
 .UNSPECIFIED.);
#727=B_SPLINE_CURVE_WITH_KNOTS('',3,(#30756,#30757,#30758,#30759,#30760,
#30761,#30762,#30763,#30764,#30765,#30766,#30767,#30768,#30769,#30770,#30771,
#30772,#30773,#30774,#30775,#30776,#30777,#30778,#30779,#30780,#30781,#30782,
#30783,#30784,#30785,#30786,#30787,#30788,#30789,#30790,#30791,#30792,#30793,
#30794,#30795,#30796,#30797,#30798,#30799,#30800,#30801,#30802,#30803,#30804,
#30805,#30806,#30807,#30808,#30809,#30810),.UNSPECIFIED.,.F.,.F.,(4,3,3,
3,3,3,3,3,3,3,3,3,3,3,3,3,3,3,4),(-0.483882268593942,-0.465763533352619,
-0.4308523820833,-0.416229812750554,-0.375093593923325,-0.358591971446984,
-0.314305820036663,-0.283376059421202,-0.270874217660563,-0.239681235538257,
-0.209721081095975,-0.19316496451099,-0.179875924603182,-0.134906943452387,
-0.112773485311706,-0.0967277413707433,-0.0829938472014202,-0.0368477058416217,
0.),.UNSPECIFIED.);
#728=B_SPLINE_CURVE_WITH_KNOTS('',3,(#32211,#32212,#32213,#32214,#32215,
#32216,#32217,#32218,#32219,#32220,#32221,#32222,#32223,#32224,#32225,#32226,
#32227,#32228,#32229,#32230,#32231,#32232,#32233,#32234,#32235,#32236,#32237,
#32238,#32239,#32240,#32241,#32242,#32243,#32244,#32245,#32246,#32247,#32248,
#32249,#32250,#32251,#32252,#32253,#32254,#32255,#32256,#32257,#32258,#32259,
#32260,#32261,#32262,#32263,#32264),.UNSPECIFIED.,.F.,.F.,(4,1,1,1,1,1,
1,1,1,1,1,1,1,1,1,1,1,1,1,1,1,1,1,1,1,1,1,1,1,1,1,1,1,1,1,1,1,1,1,1,1,1,
1,1,1,1,1,1,1,1,1,4),(0.,0.0178571428571429,0.0357142857142857,0.0535714285714286,
0.0714285714285714,0.0892857142857143,0.107142857142857,0.125,0.133928571428571,
0.138392857142857,0.142857142857143,0.166666666666667,0.19047619047619,
0.214285714285714,0.232142857142857,0.25,0.267857142857143,0.285714285714286,
0.303571428571429,0.321428571428571,0.339285714285714,0.357142857142857,
0.375,0.392857142857143,0.428571428571429,0.464285714285714,0.5,0.535714285714286,
0.553571428571429,0.571428571428571,0.589285714285714,0.607142857142857,
0.625,0.642857142857143,0.660714285714286,0.678571428571428,0.696428571428571,
0.714285714285714,0.738095238095238,0.761904761904762,0.785714285714286,
0.809523809523809,0.833333333333333,0.857142857142857,0.875,0.892857142857143,
0.910714285714286,0.928571428571429,0.946428571428571,0.964285714285714,
0.982142857142857,1.),.UNSPECIFIED.);
#729=B_SPLINE_CURVE_WITH_KNOTS('',3,(#32274,#32275,#32276,#32277,#32278,
#32279,#32280,#32281,#32282,#32283),.UNSPECIFIED.,.F.,.F.,(4,3,3,4),(-4.09254174883829,
-3.99171948725392,-2.99378961544044,-2.06514013327807),.UNSPECIFIED.);
#730=B_SPLINE_CURVE_WITH_KNOTS('',3,(#32286,#32287,#32288,#32289,#32290,
#32291,#32292),.UNSPECIFIED.,.F.,.F.,(4,3,4),(0.,0.997929871813473,1.11419103802947),
 .UNSPECIFIED.);
#731=B_SPLINE_CURVE_WITH_KNOTS('',3,(#32297,#32298,#32299,#32300,#32301,
#32302,#32303,#32304,#32305,#32306,#32307,#32308,#32309,#32310,#32311,#32312,
#32313,#32314,#32315,#32316,#32317,#32318),.UNSPECIFIED.,.F.,.F.,(4,3,3,
3,3,3,3,4),(-10.3757270560179,-9.97929871813481,-8.98136884632133,-7.98343897450785,
-6.98550910269437,-5.98757923088089,-4.98964935906741,-4.09254174883829),
 .UNSPECIFIED.);
#732=B_SPLINE_CURVE_WITH_KNOTS('',3,(#32319,#32320,#32321,#32322,#32323,
#32324,#32325,#32326,#32327,#32328,#32329,#32330,#32331,#32332,#32333,#32334,
#32335,#32336,#32337,#32338,#32339,#32340),.UNSPECIFIED.,.F.,.F.,(4,3,3,
3,3,3,3,4),(1.11419103802947,1.99585974362696,2.99378961544044,3.99171948725392,
4.9896493590674,5.98757923088088,6.98550910269437,7.39737634520906),
 .UNSPECIFIED.);
#733=B_SPLINE_CURVE_WITH_KNOTS('',3,(#32345,#32346,#32347,#32348,#32349,
#32350,#32351,#32352,#32353,#32354,#32355,#32356,#32357,#32358,#32359,#32360,
#32361,#32362,#32363,#32364,#32365,#32366),.UNSPECIFIED.,.F.,.F.,(4,3,3,
3,3,3,3,4),(-16.6589123631975,-15.9668779490157,-14.9689480772022,-13.9710182053887,
-12.9730883335753,-11.9751584617618,-10.9772285899483,-10.3757270560179),
 .UNSPECIFIED.);
#734=B_SPLINE_CURVE_WITH_KNOTS('',3,(#32367,#32368,#32369,#32370,#32371,
#32372,#32373,#32374,#32375,#32376,#32377,#32378,#32379,#32380,#32381,#32382,
#32383,#32384,#32385,#32386,#32387,#32388),.UNSPECIFIED.,.F.,.F.,(4,3,3,
3,3,3,3,4),(7.39737634520906,7.98343897450785,8.98136884632133,9.97929871813481,
10.9772285899483,11.9751584617618,12.9730883335753,13.6805616523886),
 .UNSPECIFIED.);
#735=B_SPLINE_CURVE_WITH_KNOTS('',3,(#32393,#32394,#32395,#32396,#32397,
#32398,#32399,#32400,#32401,#32402,#32403,#32404,#32405,#32406,#32407,#32408,
#32409,#32410,#32411,#32412,#32413,#32414),.UNSPECIFIED.,.F.,.F.,(4,3,3,
3,3,3,3,4),(-22.942097670377,-21.9544571798966,-20.9565273080831,-19.9585974362696,
-18.9606675644561,-17.9627376926427,-16.9648078208292,-16.6589123631975),
 .UNSPECIFIED.);
#736=B_SPLINE_CURVE_WITH_KNOTS('',3,(#32415,#32416,#32417,#32418,#32419,
#32420,#32421,#32422,#32423,#32424,#32425,#32426,#32427,#32428,#32429,#32430,
#32431,#32432,#32433,#32434,#32435,#32436,#32437,#32438,#32439),
 .UNSPECIFIED.,.F.,.F.,(4,3,3,3,3,3,3,3,4),(13.6805616523886,13.9710182053887,
14.9689480772022,15.9668779490157,16.9648078208292,17.9627376926427,18.9606675644561,
19.9585974362696,19.9637469595682),.UNSPECIFIED.);
#737=B_SPLINE_CURVE_WITH_KNOTS('',3,(#32444,#32445,#32446,#32447,#32448,
#32449,#32450,#32451,#32452,#32453,#32454,#32455,#32456,#32457,#32458,#32459,
#32460,#32461,#32462,#32463,#32464,#32465,#32466,#32467,#32468),
 .UNSPECIFIED.,.F.,.F.,(4,3,3,3,3,3,3,3,4),(-29.2252829775566,-28.9399662825909,
-27.9420364107775,-26.944106538964,-25.9461766671505,-24.948246795337,-23.9503169235235,
-22.9523870517101,-22.942097670377),.UNSPECIFIED.);
#738=B_SPLINE_CURVE_WITH_KNOTS('',3,(#32469,#32470,#32471,#32472,#32473,
#32474,#32475,#32476,#32477,#32478,#32479,#32480,#32481,#32482,#32483,#32484,
#32485,#32486,#32487,#32488,#32489,#32490),.UNSPECIFIED.,.F.,.F.,(4,3,3,
3,3,3,3,4),(19.9637469595682,20.9565273080831,21.9544571798966,22.9523870517101,
23.9503169235235,24.948246795337,25.9461766671505,26.2469322667478),
 .UNSPECIFIED.);
#739=B_SPLINE_CURVE_WITH_KNOTS('',3,(#32495,#32496,#32497,#32498,#32499,
#32500,#32501,#32502,#32503,#32504,#32505,#32506,#32507,#32508,#32509,#32510,
#32511,#32512,#32513,#32514,#32515,#32516),.UNSPECIFIED.,.F.,.F.,(4,3,3,
3,3,3,3,4),(-35.5084682847362,-34.9275455134718,-33.9296156416584,-32.9316857698449,
-31.9337558980314,-30.9358260262179,-29.9378961544044,-29.2252829775566),
 .UNSPECIFIED.);
#740=B_SPLINE_CURVE_WITH_KNOTS('',3,(#32517,#32518,#32519,#32520,#32521,
#32522,#32523,#32524,#32525,#32526,#32527,#32528,#32529,#32530,#32531,#32532,
#32533,#32534,#32535,#32536,#32537,#32538),.UNSPECIFIED.,.F.,.F.,(4,3,3,
3,3,3,3,4),(26.2469322667478,26.944106538964,27.9420364107775,28.9399662825909,
29.9378961544044,30.9358260262179,31.9337558980314,32.5301175739274),
 .UNSPECIFIED.);
#741=B_SPLINE_CURVE_WITH_KNOTS('',3,(#32543,#32544,#32545,#32546,#32547,
#32548,#32549,#32550,#32551,#32552,#32553,#32554,#32555,#32556,#32557,#32558,
#32559,#32560,#32561,#32562,#32563,#32564),.UNSPECIFIED.,.F.,.F.,(4,3,3,
3,3,3,3,4),(-41.7916535919158,-40.9151247443527,-39.9171948725392,-38.9192650007258,
-37.9213351289123,-36.9234052570988,-35.9254753852853,-35.5084682847362),
 .UNSPECIFIED.);
#742=B_SPLINE_CURVE_WITH_KNOTS('',3,(#32565,#32566,#32567,#32568,#32569,
#32570,#32571,#32572,#32573,#32574,#32575,#32576,#32577,#32578,#32579,#32580,
#32581,#32582,#32583,#32584,#32585,#32586),.UNSPECIFIED.,.F.,.F.,(4,3,3,
3,3,3,3,4),(32.5301175739274,32.9316857698449,33.9296156416584,34.9275455134718,
35.9254753852853,36.9234052570988,37.9213351289123,38.813302881107),
 .UNSPECIFIED.);
#743=B_SPLINE_CURVE_WITH_KNOTS('',3,(#32591,#32592,#32593,#32594,#32595,
#32596,#32597,#32598,#32599,#32600,#32601,#32602,#32603,#32604,#32605,#32606,
#32607,#32608,#32609,#32610,#32611,#32612,#32613,#32614,#32615),
 .UNSPECIFIED.,.F.,.F.,(4,3,3,3,3,3,3,3,4),(-48.0748388990954,-47.9006338470471,
-46.9027039752336,-45.9047741034201,-44.9068442316067,-43.9089143597932,
-42.9109844879797,-41.9130546161662,-41.7916535919158),.UNSPECIFIED.);
#744=B_SPLINE_CURVE_WITH_KNOTS('',3,(#32616,#32617,#32618,#32619,#32620,
#32621,#32622,#32623,#32624,#32625,#32626,#32627,#32628,#32629,#32630,#32631,
#32632,#32633,#32634,#32635,#32636,#32637,#32638,#32639,#32640),
 .UNSPECIFIED.,.F.,.F.,(4,3,3,3,3,3,3,3,4),(38.813302881107,38.9192650007258,
39.9171948725392,40.9151247443527,41.9130546161662,42.9109844879797,43.9089143597932,
44.9068442316066,45.0964881882866),.UNSPECIFIED.);
#745=B_SPLINE_CURVE_WITH_KNOTS('',3,(#32645,#32646,#32647,#32648,#32649,
#32650,#32651,#32652,#32653,#32654,#32655,#32656,#32657,#32658,#32659,#32660,
#32661,#32662,#32663,#32664,#32665,#32666),.UNSPECIFIED.,.F.,.F.,(4,3,3,
3,3,3,3,4),(-54.358024206275,-53.888213077928,-52.8902832061145,-51.892353334301,
-50.8944234624875,-49.8964935906741,-48.8985637188606,-48.0748388990954),
 .UNSPECIFIED.);
#746=B_SPLINE_CURVE_WITH_KNOTS('',3,(#32667,#32668,#32669,#32670,#32671,
#32672,#32673,#32674,#32675,#32676,#32677,#32678,#32679,#32680,#32681,#32682,
#32683,#32684,#32685,#32686,#32687,#32688),.UNSPECIFIED.,.F.,.F.,(4,3,3,
3,3,3,3,4),(45.0964881882866,45.9047741034201,46.9027039752336,47.9006338470471,
48.8985637188606,49.8964935906741,50.8944234624875,51.3796734954662),
 .UNSPECIFIED.);
#747=B_SPLINE_CURVE_WITH_KNOTS('',3,(#32693,#32694,#32695,#32696,#32697,
#32698,#32699,#32700,#32701,#32702,#32703,#32704,#32705,#32706,#32707,#32708,
#32709,#32710,#32711,#32712,#32713,#32714),.UNSPECIFIED.,.F.,.F.,(4,3,3,
3,3,3,3,4),(-60.6412095134546,-59.8757923088089,-58.8778624369954,-57.8799325651819,
-56.8820026933684,-55.8840728215549,-54.8861429497415,-54.358024206275),
 .UNSPECIFIED.);
#748=B_SPLINE_CURVE_WITH_KNOTS('',3,(#32715,#32716,#32717,#32718,#32719,
#32720,#32721,#32722,#32723,#32724,#32725,#32726,#32727,#32728,#32729,#32730,
#32731,#32732,#32733,#32734,#32735,#32736),.UNSPECIFIED.,.F.,.F.,(4,3,3,
3,3,3,3,4),(51.3796734954662,51.892353334301,52.8902832061145,53.888213077928,
54.8861429497415,55.8840728215549,56.8820026933684,57.6628588026458),
 .UNSPECIFIED.);
#749=B_SPLINE_CURVE_WITH_KNOTS('',3,(#32741,#32742,#32743,#32744,#32745,
#32746,#32747,#32748,#32749,#32750,#32751,#32752,#32753,#32754,#32755,#32756,
#32757,#32758,#32759,#32760,#32761,#32762,#32763,#32764,#32765),
 .UNSPECIFIED.,.F.,.F.,(4,3,3,3,3,3,3,3,4),(-66.9243948206342,-66.8613014115032,
-65.8633715396898,-64.8654416678763,-63.8675117960628,-62.8695819242493,
-61.8716520524358,-60.8737221806224,-60.6412095134546),.UNSPECIFIED.);
#750=B_SPLINE_CURVE_WITH_KNOTS('',3,(#32766,#32767,#32768,#32769,#32770,
#32771,#32772,#32773,#32774,#32775,#32776,#32777,#32778,#32779,#32780,#32781,
#32782,#32783,#32784,#32785,#32786,#32787,#32788,#32789,#32790),
 .UNSPECIFIED.,.F.,.F.,(4,3,3,3,3,3,3,3,4),(57.6628588026458,57.8799325651819,
58.8778624369954,59.8757923088089,60.8737221806224,61.8716520524358,62.8695819242493,
63.8675117960628,63.9460441098254),.UNSPECIFIED.);
#751=B_SPLINE_CURVE_WITH_KNOTS('',3,(#32795,#32796,#32797,#32798,#32799,
#32800,#32801,#32802,#32803,#32804,#32805,#32806,#32807,#32808,#32809,#32810,
#32811,#32812,#32813,#32814,#32815,#32816),.UNSPECIFIED.,.F.,.F.,(4,3,3,
3,3,3,3,4),(-73.2075801278138,-72.8488806423841,-71.8509507705706,-70.8530208987571,
-69.8550910269437,-68.8571611551302,-67.8592312833167,-66.9243948206342),
 .UNSPECIFIED.);
#752=B_SPLINE_CURVE_WITH_KNOTS('',3,(#32817,#32818,#32819,#32820,#32821,
#32822,#32823,#32824,#32825,#32826,#32827,#32828,#32829,#32830,#32831,#32832,
#32833,#32834,#32835,#32836,#32837,#32838),.UNSPECIFIED.,.F.,.F.,(4,3,3,
3,3,3,3,4),(63.9460441098254,64.8654416678763,65.8633715396898,66.8613014115032,
67.8592312833167,68.8571611551302,69.8550910269437,70.229229417005),
 .UNSPECIFIED.);
#753=B_SPLINE_CURVE_WITH_KNOTS('',3,(#32843,#32844,#32845,#32846,#32847,
#32848,#32849,#32850,#32851,#32852,#32853,#32854,#32855,#32856,#32857,#32858,
#32859,#32860,#32861,#32862,#32863,#32864),.UNSPECIFIED.,.F.,.F.,(4,3,3,
3,3,3,3,4),(-79.4907654349934,-78.836459873265,-77.8385300014515,-76.840600129638,
-75.8426702578246,-74.8447403860111,-73.8468105141976,-73.2075801278138),
 .UNSPECIFIED.);
#754=B_SPLINE_CURVE_WITH_KNOTS('',3,(#32865,#32866,#32867,#32868,#32869,
#32870,#32871,#32872,#32873,#32874,#32875,#32876,#32877,#32878,#32879,#32880,
#32881,#32882,#32883,#32884,#32885,#32886),.UNSPECIFIED.,.F.,.F.,(4,3,3,
3,3,3,3,4),(70.229229417005,70.8530208987571,71.8509507705706,72.8488806423841,
73.8468105141976,74.8447403860111,75.8426702578246,76.5124147241846),
 .UNSPECIFIED.);
#755=B_SPLINE_CURVE_WITH_KNOTS('',3,(#32891,#32892,#32893,#32894,#32895,
#32896,#32897,#32898,#32899,#32900,#32901,#32902,#32903,#32904,#32905,#32906,
#32907,#32908,#32909,#32910,#32911,#32912),.UNSPECIFIED.,.F.,.F.,(4,3,3,
3,3,3,3,4),(-85.773950742173,-84.8240391041459,-83.8261092323324,-82.8281793605189,
-81.8302494887054,-80.832319616892,-79.8343897450785,-79.4907654349934),
 .UNSPECIFIED.);
#756=B_SPLINE_CURVE_WITH_KNOTS('',3,(#32913,#32914,#32915,#32916,#32917,
#32918,#32919,#32920,#32921,#32922,#32923,#32924,#32925,#32926,#32927,#32928,
#32929,#32930,#32931,#32932,#32933,#32934),.UNSPECIFIED.,.F.,.F.,(4,3,3,
3,3,3,3,4),(76.5124147241846,76.840600129638,77.8385300014515,78.836459873265,
79.8343897450785,80.832319616892,81.8302494887054,82.7956000313641),
 .UNSPECIFIED.);
#757=B_SPLINE_CURVE_WITH_KNOTS('',3,(#32939,#32940,#32941,#32942,#32943,
#32944,#32945,#32946,#32947,#32948,#32949,#32950,#32951,#32952,#32953,#32954,
#32955,#32956,#32957,#32958,#32959,#32960,#32961,#32962,#32963),
 .UNSPECIFIED.,.F.,.F.,(4,3,3,3,3,3,3,3,4),(-92.0571360493526,-91.8095482068402,
-90.8116183350268,-89.8136884632133,-88.8157585913998,-87.8178287195863,
-86.8198988477728,-85.8219689759594,-85.773950742173),.UNSPECIFIED.);
#758=B_SPLINE_CURVE_WITH_KNOTS('',3,(#32964,#32965,#32966,#32967,#32968,
#32969,#32970,#32971,#32972,#32973,#32974,#32975,#32976,#32977,#32978,#32979,
#32980,#32981,#32982,#32983,#32984,#32985,#32986,#32987,#32988),
 .UNSPECIFIED.,.F.,.F.,(4,3,3,3,3,3,3,3,4),(82.7956000313641,82.8281793605189,
83.8261092323324,84.8240391041459,85.8219689759594,86.8198988477728,87.8178287195863,
88.8157585913998,89.0787853385437),.UNSPECIFIED.);
#759=B_SPLINE_CURVE_WITH_KNOTS('',3,(#32993,#32994,#32995,#32996,#32997,
#32998,#32999,#33000,#33001,#33002,#33003,#33004,#33005,#33006,#33007,#33008,
#33009,#33010,#33011,#33012,#33013,#33014),.UNSPECIFIED.,.F.,.F.,(4,3,3,
3,3,3,3,4),(-98.3403213565322,-97.7971274377211,-96.7991975659076,-95.8012676940942,
-94.8033378222807,-93.8054079504672,-92.8074780786537,-92.0571360493526),
 .UNSPECIFIED.);
#760=B_SPLINE_CURVE_WITH_KNOTS('',3,(#33015,#33016,#33017,#33018,#33019,
#33020,#33021,#33022,#33023,#33024,#33025,#33026,#33027,#33028,#33029,#33030,
#33031,#33032,#33033,#33034,#33035,#33036),.UNSPECIFIED.,.F.,.F.,(4,3,3,
3,3,3,3,4),(89.0787853385437,89.8136884632133,90.8116183350268,91.8095482068402,
92.8074780786537,93.8054079504672,94.8033378222807,95.3619706457233),
 .UNSPECIFIED.);
#761=B_SPLINE_CURVE_WITH_KNOTS('',3,(#33041,#33042,#33043,#33044,#33045,
#33046,#33047,#33048,#33049,#33050,#33051,#33052,#33053,#33054,#33055,#33056,
#33057,#33058,#33059,#33060,#33061,#33062),.UNSPECIFIED.,.F.,.F.,(4,3,3,
3,3,3,3,4),(-104.623506663712,-103.784706668602,-102.786776796789,-101.788846924975,
-100.790917053162,-99.7929871813481,-98.7950573095346,-98.3403213565322),
 .UNSPECIFIED.);
#762=B_SPLINE_CURVE_WITH_KNOTS('',3,(#33063,#33064,#33065,#33066,#33067,
#33068,#33069,#33070,#33071,#33072,#33073,#33074,#33075,#33076,#33077,#33078,
#33079,#33080,#33081,#33082,#33083,#33084),.UNSPECIFIED.,.F.,.F.,(4,3,3,
3,3,3,3,4),(95.3619706457233,95.8012676940942,96.7991975659077,97.7971274377211,
98.7950573095346,99.7929871813481,100.790917053162,101.645155952903),
 .UNSPECIFIED.);
#763=B_SPLINE_CURVE_WITH_KNOTS('',3,(#33089,#33090,#33091,#33092,#33093,
#33094,#33095,#33096,#33097,#33098,#33099,#33100,#33101,#33102,#33103,#33104,
#33105,#33106,#33107,#33108,#33109,#33110,#33111,#33112,#33113),
 .UNSPECIFIED.,.F.,.F.,(4,3,3,3,3,3,3,3,4),(-110.906691970891,-110.770215771296,
-109.772285899483,-108.774356027669,-107.776426155856,-106.778496284042,
-105.780566412229,-104.782636540416,-104.623506663712),.UNSPECIFIED.);
#764=B_SPLINE_CURVE_WITH_KNOTS('',3,(#33114,#33115,#33116,#33117,#33118,
#33119,#33120,#33121,#33122,#33123,#33124,#33125,#33126,#33127,#33128,#33129,
#33130,#33131,#33132,#33133,#33134,#33135,#33136,#33137,#33138),
 .UNSPECIFIED.,.F.,.F.,(4,3,3,3,3,3,3,3,4),(101.645155952903,101.788846924975,
102.786776796789,103.784706668602,104.782636540416,105.780566412229,106.778496284042,
107.776426155856,107.928341260083),.UNSPECIFIED.);
#765=B_SPLINE_CURVE_WITH_KNOTS('',3,(#33143,#33144,#33145,#33146,#33147,
#33148,#33149,#33150,#33151,#33152,#33153,#33154,#33155,#33156,#33157,#33158,
#33159,#33160,#33161,#33162,#33163,#33164),.UNSPECIFIED.,.F.,.F.,(4,3,3,
3,3,3,3,4),(-117.189877278071,-116.757795002177,-115.759865130364,-114.76193525855,
-113.764005386737,-112.766075514923,-111.76814564311,-110.906691970891),
 .UNSPECIFIED.);
#766=B_SPLINE_CURVE_WITH_KNOTS('',3,(#33165,#33166,#33167,#33168,#33169,
#33170,#33171,#33172,#33173,#33174,#33175,#33176,#33177,#33178,#33179,#33180,
#33181,#33182,#33183,#33184,#33185,#33186),.UNSPECIFIED.,.F.,.F.,(4,3,3,
3,3,3,3,4),(107.928341260083,108.774356027669,109.772285899483,110.770215771296,
111.76814564311,112.766075514923,113.764005386737,114.211526567262),
 .UNSPECIFIED.);
#767=B_SPLINE_CURVE_WITH_KNOTS('',3,(#33191,#33192,#33193,#33194,#33195,
#33196,#33197,#33198,#33199,#33200,#33201,#33202,#33203,#33204,#33205,#33206,
#33207,#33208,#33209,#33210,#33211,#33212),.UNSPECIFIED.,.F.,.F.,(4,3,3,
3,3,3,3,4),(-123.473062585251,-122.745374233058,-121.747444361245,-120.749514489431,
-119.751584617618,-118.753654745804,-117.755724873991,-117.189877278071),
 .UNSPECIFIED.);
#768=B_SPLINE_CURVE_WITH_KNOTS('',3,(#33213,#33214,#33215,#33216,#33217,
#33218,#33219,#33220,#33221,#33222,#33223,#33224,#33225,#33226,#33227,#33228,
#33229,#33230,#33231,#33232,#33233,#33234),.UNSPECIFIED.,.F.,.F.,(4,3,3,
3,3,3,3,4),(114.211526567262,114.76193525855,115.759865130364,116.757795002177,
117.755724873991,118.753654745804,119.751584617618,120.494711874442),
 .UNSPECIFIED.);
#769=B_SPLINE_CURVE_WITH_KNOTS('',3,(#33239,#33240,#33241,#33242,#33243,
#33244,#33245,#33246,#33247,#33248,#33249,#33250,#33251,#33252,#33253,#33254,
#33255,#33256,#33257,#33258,#33259,#33260,#33261,#33262,#33263),
 .UNSPECIFIED.,.F.,.F.,(4,3,3,3,3,3,3,3,4),(-129.75624789243,-129.730883335753,
-128.732953463939,-127.735023592126,-126.737093720312,-125.739163848499,
-124.741233976685,-123.743304104872,-123.473062585251),.UNSPECIFIED.);
#770=B_SPLINE_CURVE_WITH_KNOTS('',3,(#33264,#33265,#33266,#33267,#33268,
#33269,#33270,#33271,#33272,#33273,#33274,#33275,#33276,#33277,#33278,#33279,
#33280,#33281,#33282,#33283,#33284,#33285,#33286,#33287,#33288),
 .UNSPECIFIED.,.F.,.F.,(4,3,3,3,3,3,3,3,4),(120.494711874442,120.749514489431,
121.747444361245,122.745374233058,123.743304104872,124.741233976685,125.739163848499,
126.737093720312,126.777897181621),.UNSPECIFIED.);
#771=B_SPLINE_CURVE_WITH_KNOTS('',3,(#33293,#33294,#33295,#33296,#33297,
#33298,#33299,#33300,#33301,#33302,#33303,#33304,#33305,#33306,#33307,#33308,
#33309,#33310,#33311,#33312,#33313,#33314),.UNSPECIFIED.,.F.,.F.,(4,3,3,
3,3,3,3,4),(-136.03943319961,-135.718462566633,-134.72053269482,-133.722602823006,
-132.724672951193,-131.72674307938,-130.728813207566,-129.75624789243),
 .UNSPECIFIED.);
#772=B_SPLINE_CURVE_WITH_KNOTS('',3,(#33315,#33316,#33317,#33318,#33319,
#33320,#33321,#33322,#33323,#33324,#33325,#33326,#33327,#33328,#33329,#33330,
#33331,#33332,#33333,#33334,#33335,#33336),.UNSPECIFIED.,.F.,.F.,(4,3,3,
3,3,3,3,4),(126.777897181621,127.735023592126,128.732953463939,129.730883335753,
130.728813207566,131.72674307938,132.724672951193,133.061082488801),
 .UNSPECIFIED.);
#773=B_SPLINE_CURVE_WITH_KNOTS('',3,(#33342,#33343,#33344,#33345,#33346,
#33347),.UNSPECIFIED.,.F.,.F.,(4,1,1,4),(147.65485471872,148.331813957558,
149.329743829371,150.258393311533),.UNSPECIFIED.);
#774=B_SPLINE_CURVE_WITH_KNOTS('',3,(#33350,#33351,#33352,#33353,#33354),
 .UNSPECIFIED.,.F.,.F.,(4,1,4),(147.65485471872,148.020768976627,149.018698848441),
 .UNSPECIFIED.);
#775=B_SPLINE_CURVE_WITH_KNOTS('',3,(#33359,#33360,#33361,#33362,#33363,
#33364,#33365,#33366,#33367,#33368),.UNSPECIFIED.,.F.,.F.,(4,1,1,1,1,1,
1,4),(141.371669411541,142.344234726677,143.34216459849,144.340094470304,
145.338024342117,146.335954213931,147.333884085744,147.65485471872),
 .UNSPECIFIED.);
#776=B_SPLINE_CURVE_WITH_KNOTS('',3,(#33369,#33370,#33371,#33372,#33373,
#33374,#33375,#33376,#33377,#33378),.UNSPECIFIED.,.F.,.F.,(4,1,1,1,1,1,
1,4),(141.371669411541,142.033189745746,143.03111961756,144.029049489373,
145.026979361187,146.024909233,147.022839104814,147.65485471872),
 .UNSPECIFIED.);
#777=B_SPLINE_CURVE_WITH_KNOTS('',3,(#33383,#33384,#33385,#33386,#33387,
#33388,#33389,#33390,#33391,#33392,#33393),.UNSPECIFIED.,.F.,.F.,(4,1,1,
1,1,1,1,1,4),(135.088484104361,135.358725623982,136.356655495796,137.354585367609,
138.352515239423,139.350445111236,140.34837498305,141.346304854863,141.371669411541),
 .UNSPECIFIED.);
#778=B_SPLINE_CURVE_WITH_KNOTS('',3,(#33394,#33395,#33396,#33397,#33398,
#33399,#33400,#33401,#33402,#33403),.UNSPECIFIED.,.F.,.F.,(4,1,1,1,1,1,
1,4),(135.088484104361,136.045610514865,137.043540386679,138.041470258492,
139.039400130306,140.037330002119,141.035259873933,141.371669411541),
 .UNSPECIFIED.);
#779=B_SPLINE_CURVE_WITH_KNOTS('',3,(#33408,#33409,#33410,#33411,#33412,
#33413,#33414,#33415,#33416,#33417),.UNSPECIFIED.,.F.,.F.,(4,1,1,1,1,1,
1,4),(128.805298797182,129.371146393101,130.369076264915,131.367006136728,
132.364936008542,133.362865880355,134.360795752169,135.088484104361),
 .UNSPECIFIED.);
#780=B_SPLINE_CURVE_WITH_KNOTS('',3,(#33418,#33419,#33420,#33421,#33422,
#33423,#33424,#33425,#33426,#33427,#33428),.UNSPECIFIED.,.F.,.F.,(4,1,1,
1,1,1,1,1,4),(128.805298797182,129.060101412171,130.058031283984,131.055961155798,
132.053891027611,133.051820899425,134.049750771238,135.047680643052,135.088484104361),
 .UNSPECIFIED.);
#781=B_SPLINE_CURVE_WITH_KNOTS('',3,(#33433,#33434,#33435,#33436,#33437,
#33438,#33439,#33440,#33441,#33442),.UNSPECIFIED.,.F.,.F.,(4,1,1,1,1,1,
1,4),(122.522113490002,123.383567162221,124.381497034034,125.379426905847,
126.377356777661,127.375286649474,128.373216521288,128.805298797182),
 .UNSPECIFIED.);
#782=B_SPLINE_CURVE_WITH_KNOTS('',3,(#33443,#33444,#33445,#33446,#33447,
#33448,#33449,#33450,#33451,#33452),.UNSPECIFIED.,.F.,.F.,(4,1,1,1,1,1,
1,4),(122.522113490002,123.07252218129,124.070452053104,125.068381924917,
126.066311796731,127.064241668544,128.062171540357,128.805298797182),
 .UNSPECIFIED.);
#783=B_SPLINE_CURVE_WITH_KNOTS('',3,(#33457,#33458,#33459,#33460,#33461,
#33462,#33463,#33464,#33465,#33466,#33467),.UNSPECIFIED.,.F.,.F.,(4,1,1,
1,1,1,1,1,4),(116.238928182822,116.398058059526,117.39598793134,118.393917803153,
119.391847674967,120.38977754678,121.387707418594,122.385637290407,122.522113490002),
 .UNSPECIFIED.);
#784=B_SPLINE_CURVE_WITH_KNOTS('',3,(#33468,#33469,#33470,#33471,#33472,
#33473,#33474,#33475,#33476,#33477),.UNSPECIFIED.,.F.,.F.,(4,1,1,1,1,1,
1,4),(116.238928182822,117.084942950409,118.082872822223,119.080802694036,
120.07873256585,121.076662437663,122.074592309477,122.522113490002),
 .UNSPECIFIED.);
#785=B_SPLINE_CURVE_WITH_KNOTS('',3,(#33482,#33483,#33484,#33485,#33486,
#33487,#33488,#33489,#33490,#33491),.UNSPECIFIED.,.F.,.F.,(4,1,1,1,1,1,
1,4),(109.955742875643,110.410478828645,111.408408700459,112.406338572272,
113.404268444086,114.402198315899,115.400128187713,116.238928182822),
 .UNSPECIFIED.);
#786=B_SPLINE_CURVE_WITH_KNOTS('',3,(#33492,#33493,#33494,#33495,#33496,
#33497,#33498,#33499,#33500,#33501,#33502),.UNSPECIFIED.,.F.,.F.,(4,1,1,
1,1,1,1,1,4),(109.955742875643,110.099433847715,111.097363719528,112.095293591342,
113.093223463155,114.091153334969,115.089083206782,116.087013078596,116.238928182822),
 .UNSPECIFIED.);
#787=B_SPLINE_CURVE_WITH_KNOTS('',3,(#33507,#33508,#33509,#33510,#33511,
#33512,#33513,#33514,#33515,#33516),.UNSPECIFIED.,.F.,.F.,(4,1,1,1,1,1,
1,4),(103.672557568463,104.422899597764,105.420829469578,106.418759341391,
107.416689213205,108.414619085018,109.412548956832,109.955742875643),
 .UNSPECIFIED.);
#788=B_SPLINE_CURVE_WITH_KNOTS('',3,(#33517,#33518,#33519,#33520,#33521,
#33522,#33523,#33524,#33525,#33526),.UNSPECIFIED.,.F.,.F.,(4,1,1,1,1,1,
1,4),(103.672557568463,104.111854616834,105.109784488647,106.107714360461,
107.105644232274,108.103574104088,109.101503975901,109.955742875643),
 .UNSPECIFIED.);
#789=B_SPLINE_CURVE_WITH_KNOTS('',3,(#33531,#33532,#33533,#33534,#33535,
#33536,#33537,#33538,#33539,#33540,#33541),.UNSPECIFIED.,.F.,.F.,(4,1,1,
1,1,1,1,1,4),(97.3893722612836,97.43739049507,98.4353203668835,99.433250238697,
100.43118011051,101.429109982324,102.427039854137,103.424969725951,103.672557568463),
 .UNSPECIFIED.);
#790=B_SPLINE_CURVE_WITH_KNOTS('',3,(#33542,#33543,#33544,#33545,#33546,
#33547,#33548,#33549,#33550,#33551),.UNSPECIFIED.,.F.,.F.,(4,1,1,1,1,1,
1,4),(97.3893722612836,98.1242753859531,99.1222052577666,100.12013512958,
101.118065001394,102.115994873207,103.11392474502,103.672557568463),
 .UNSPECIFIED.);
#791=B_SPLINE_CURVE_WITH_KNOTS('',3,(#33556,#33557,#33558,#33559,#33560,
#33561,#33562,#33563,#33564,#33565),.UNSPECIFIED.,.F.,.F.,(4,1,1,1,1,1,
1,4),(91.106186954104,91.4498112641891,92.4477411360026,93.4456710078161,
94.4436008796296,95.441530751443,96.4394606232565,97.3893722612836),
 .UNSPECIFIED.);
#792=B_SPLINE_CURVE_WITH_KNOTS('',3,(#33566,#33567,#33568,#33569,#33570,
#33571,#33572,#33573,#33574,#33575,#33576),.UNSPECIFIED.,.F.,.F.,(4,1,1,
1,1,1,1,1,4),(91.106186954104,91.1387662832587,92.1366961550722,93.1346260268857,
94.1325558986991,95.1304857705126,96.1284156423261,97.1263455141396,97.3893722612836),
 .UNSPECIFIED.);
#793=B_SPLINE_CURVE_WITH_KNOTS('',3,(#33581,#33582,#33583,#33584,#33585,
#33586,#33587,#33588,#33589,#33590),.UNSPECIFIED.,.F.,.F.,(4,1,1,1,1,1,
1,4),(84.8230016469244,85.4622320333082,86.4601619051217,87.4580917769352,
88.4560216487487,89.4539515205621,90.4518813923756,91.106186954104),
 .UNSPECIFIED.);
#794=B_SPLINE_CURVE_WITH_KNOTS('',3,(#33591,#33592,#33593,#33594,#33595,
#33596,#33597,#33598,#33599,#33600),.UNSPECIFIED.,.F.,.F.,(4,1,1,1,1,1,
1,4),(84.8230016469244,85.1511870523778,86.1491169241913,87.1470467960048,
88.1449766678183,89.1429065396317,90.1408364114452,91.106186954104),
 .UNSPECIFIED.);
#795=B_SPLINE_CURVE_WITH_KNOTS('',3,(#33605,#33606,#33607,#33608,#33609,
#33610,#33611,#33612,#33613,#33614),.UNSPECIFIED.,.F.,.F.,(4,1,1,1,1,1,
1,4),(78.5398163397449,79.4746528024273,80.4725826742408,81.4705125460543,
82.4684424178678,83.4663722896813,84.4643021614947,84.8230016469244),
 .UNSPECIFIED.);
#796=B_SPLINE_CURVE_WITH_KNOTS('',3,(#33615,#33616,#33617,#33618,#33619,
#33620,#33621,#33622,#33623,#33624),.UNSPECIFIED.,.F.,.F.,(4,1,1,1,1,1,
1,4),(78.5398163397449,79.1636078214969,80.1615376933104,81.1594675651239,
82.1573974369374,83.1553273087509,84.1532571805643,84.8230016469244),
 .UNSPECIFIED.);
#797=B_SPLINE_CURVE_WITH_KNOTS('',3,(#33629,#33630,#33631,#33632,#33633,
#33634,#33635,#33636,#33637,#33638,#33639),.UNSPECIFIED.,.F.,.F.,(4,1,1,
1,1,1,1,1,4),(72.2566310325653,72.489143699733,73.4870735715464,74.4850034433599,
75.4829333151734,76.4808631869869,77.4787930588004,78.4767229306139,78.5398163397449),
 .UNSPECIFIED.);
#798=B_SPLINE_CURVE_WITH_KNOTS('',3,(#33640,#33641,#33642,#33643,#33644,
#33645,#33646,#33647,#33648,#33649),.UNSPECIFIED.,.F.,.F.,(4,1,1,1,1,1,
1,4),(72.2566310325653,73.176028590616,74.1739584624295,75.171888334243,
76.1698182060565,77.16774807787,78.1656779496834,78.5398163397449),
 .UNSPECIFIED.);
#799=B_SPLINE_CURVE_WITH_KNOTS('',3,(#33654,#33655,#33656,#33657,#33658,
#33659,#33660,#33661,#33662,#33663),.UNSPECIFIED.,.F.,.F.,(4,1,1,1,1,1,
1,4),(65.9734457253856,66.5015644688521,67.4994943406656,68.497424212479,
69.4953540842925,70.493283956106,71.4912138279195,72.2566310325653),
 .UNSPECIFIED.);
#800=B_SPLINE_CURVE_WITH_KNOTS('',3,(#33664,#33665,#33666,#33667,#33668,
#33669,#33670,#33671,#33672,#33673,#33674),.UNSPECIFIED.,.F.,.F.,(4,1,1,
1,1,1,1,1,4),(65.9734457253856,66.1905194879217,67.1884493597351,68.1863792315486,
69.1843091033621,70.1822389751756,71.1801688469891,72.1780987188026,72.2566310325653),
 .UNSPECIFIED.);
#801=B_SPLINE_CURVE_WITH_KNOTS('',3,(#33679,#33680,#33681,#33682,#33683,
#33684,#33685,#33686,#33687,#33688),.UNSPECIFIED.,.F.,.F.,(4,1,1,1,1,1,
1,4),(59.6902604182061,60.5139852379712,61.5119151097847,62.5098449815982,
63.5077748534116,64.5057047252251,65.5036345970386,65.9734457253856),
 .UNSPECIFIED.);
#802=B_SPLINE_CURVE_WITH_KNOTS('',3,(#33689,#33690,#33691,#33692,#33693,
#33694,#33695,#33696,#33697,#33698),.UNSPECIFIED.,.F.,.F.,(4,1,1,1,1,1,
1,4),(59.6902604182061,60.2029402570408,61.2008701288543,62.1988000006677,
63.1967298724812,64.1946597442947,65.1925896161082,65.9734457253856),
 .UNSPECIFIED.);
#803=B_SPLINE_CURVE_WITH_KNOTS('',3,(#33703,#33704,#33705,#33706,#33707,
#33708,#33709,#33710,#33711,#33712,#33713),.UNSPECIFIED.,.F.,.F.,(4,1,1,
1,1,1,1,1,4),(53.4070751110265,53.5284761352768,54.5264060070903,55.5243358789038,
56.5222657507173,57.5201956225308,58.5181254943442,59.5160553661577,59.6902604182061),
 .UNSPECIFIED.);
#804=B_SPLINE_CURVE_WITH_KNOTS('',3,(#33714,#33715,#33716,#33717,#33718,
#33719,#33720,#33721,#33722,#33723),.UNSPECIFIED.,.F.,.F.,(4,1,1,1,1,1,
1,4),(53.4070751110265,54.2153610261599,55.2132908979734,56.2112207697869,
57.2091506416003,58.2070805134138,59.2050103852273,59.6902604182061),
 .UNSPECIFIED.);
#805=B_SPLINE_CURVE_WITH_KNOTS('',3,(#33728,#33729,#33730,#33731,#33732,
#33733,#33734,#33735,#33736,#33737),.UNSPECIFIED.,.F.,.F.,(4,1,1,1,1,1,
1,4),(47.1238898038469,47.540896904396,48.5388267762094,49.5367566480229,
50.5346865198364,51.5326163916499,52.5305462634634,53.4070751110265),
 .UNSPECIFIED.);
#806=B_SPLINE_CURVE_WITH_KNOTS('',3,(#33738,#33739,#33740,#33741,#33742,
#33743,#33744,#33745,#33746,#33747,#33748),.UNSPECIFIED.,.F.,.F.,(4,1,1,
1,1,1,1,1,4),(47.1238898038469,47.2298519234655,48.227781795279,49.2257116670925,
50.223641538906,51.2215714107194,52.2195012825329,53.2174311543464,53.4070751110265),
 .UNSPECIFIED.);
#807=B_SPLINE_CURVE_WITH_KNOTS('',3,(#33753,#33754,#33755,#33756,#33757,
#33758,#33759,#33760,#33761,#33762),.UNSPECIFIED.,.F.,.F.,(4,1,1,1,1,1,
1,4),(40.8407044966673,41.5533176735151,42.5512475453285,43.549177417142,
44.5471072889555,45.545037160769,46.5429670325825,47.1238898038469),
 .UNSPECIFIED.);
#808=B_SPLINE_CURVE_WITH_KNOTS('',3,(#33763,#33764,#33765,#33766,#33767,
#33768,#33769,#33770,#33771,#33772),.UNSPECIFIED.,.F.,.F.,(4,1,1,1,1,1,
1,4),(40.8407044966673,41.2422726925846,42.2402025643981,43.2381324362116,
44.2360623080251,45.2339921798386,46.231922051652,47.1238898038469),
 .UNSPECIFIED.);
#809=B_SPLINE_CURVE_WITH_KNOTS('',3,(#33777,#33778,#33779,#33780,#33781,
#33782,#33783,#33784,#33785,#33786,#33787),.UNSPECIFIED.,.F.,.F.,(4,1,1,
1,1,1,1,1,4),(34.5575191894877,34.5678085708207,35.5657384426342,36.5636683144477,
37.5615981862611,38.5595280580746,39.5574579298881,40.5553878017016,40.8407044966673),
 .UNSPECIFIED.);
#810=B_SPLINE_CURVE_WITH_KNOTS('',3,(#33788,#33789,#33790,#33791,#33792,
#33793,#33794,#33795,#33796,#33797),.UNSPECIFIED.,.F.,.F.,(4,1,1,1,1,1,
1,4),(34.5575191894877,35.2546934617038,36.2526233335172,37.2505532053307,
38.2484830771442,39.2464129489577,40.2443428207712,40.8407044966673),
 .UNSPECIFIED.);
#811=B_SPLINE_CURVE_WITH_KNOTS('',3,(#33802,#33803,#33804,#33805,#33806,
#33807,#33808,#33809,#33810,#33811),.UNSPECIFIED.,.F.,.F.,(4,1,1,1,1,1,
1,4),(28.2743338823081,28.5802293399398,29.5781592117533,30.5760890835668,
31.5740189553803,32.5719488271937,33.5698786990072,34.5575191894877),
 .UNSPECIFIED.);
#812=B_SPLINE_CURVE_WITH_KNOTS('',3,(#33812,#33813,#33814,#33815,#33816,
#33817,#33818,#33819,#33820,#33821),.UNSPECIFIED.,.F.,.F.,(4,1,1,1,1,1,
1,4),(28.2743338823081,29.2671142308229,30.2650441026364,31.2629739744498,
32.2609038462633,33.2588337180768,34.2567635898903,34.5575191894877),
 .UNSPECIFIED.);
#813=B_SPLINE_CURVE_WITH_KNOTS('',3,(#33826,#33827,#33828,#33829,#33830,
#33831,#33832,#33833,#33834,#33835),.UNSPECIFIED.,.F.,.F.,(4,1,1,1,1,1,
1,4),(21.9911485751285,22.5926501090589,23.5905799808724,24.5885098526859,
25.5864397244994,26.5843695963128,27.5822994681263,28.2743338823081),
 .UNSPECIFIED.);
#814=B_SPLINE_CURVE_WITH_KNOTS('',3,(#33836,#33837,#33838,#33839,#33840,
#33841,#33842,#33843,#33844,#33845,#33846),.UNSPECIFIED.,.F.,.F.,(4,1,1,
1,1,1,1,1,4),(21.9911485751285,22.2816051281285,23.279534999942,24.2774648717555,
25.2753947435689,26.2733246153824,27.2712544871959,28.2691843590094,28.2743338823081),
 .UNSPECIFIED.);
#815=B_SPLINE_CURVE_WITH_KNOTS('',3,(#33851,#33852,#33853,#33854,#33855,
#33856,#33857,#33858,#33859,#33860),.UNSPECIFIED.,.F.,.F.,(4,1,1,1,1,1,
1,4),(15.7079632679489,16.605070878178,17.6030007499915,18.600930621805,
19.5988604936185,20.596790365432,21.5947202372454,21.9911485751285),
 .UNSPECIFIED.);
#816=B_SPLINE_CURVE_WITH_KNOTS('',3,(#33861,#33862,#33863,#33864,#33865,
#33866,#33867,#33868,#33869,#33870),.UNSPECIFIED.,.F.,.F.,(4,1,1,1,1,1,
1,4),(15.7079632679489,16.2940258972476,17.2919557690611,18.2898856408746,
19.2878155126881,20.2857453845015,21.283675256315,21.9911485751285),
 .UNSPECIFIED.);
#817=B_SPLINE_CURVE_WITH_KNOTS('',3,(#33873,#33874,#33875,#33876,#33877,
#33878,#33879,#33880,#33881,#33882,#33883,#33884,#33885,#33886,#33887,#33888,
#33889,#33890,#33891,#33892,#33893,#33894,#33895,#33896,#33897,#33898,#33899,
#33900,#33901,#33902,#33903,#33904,#33905,#33906,#33907,#33908,#33909,#33910,
#33911,#33912,#33913,#33914,#33915,#33916,#33917,#33918,#33919,#33920,#33921,
#33922,#33923,#33924),.UNSPECIFIED.,.F.,.F.,(4,3,3,3,3,3,3,3,3,3,3,3,3,
3,3,3,3,4),(-0.366397579005835,-0.355436711127808,-0.328765885113455,-0.316053385254379,
-0.292504079879806,-0.280231653992808,-0.245255630742482,-0.21857122152355,
-0.207922214642856,-0.187195667096964,-0.163796208709843,-0.149553713974392,
-0.138748641693171,-0.104061481269878,-0.0827650289191262,-0.0667799803750929,
-0.0282862380303849,0.),.UNSPECIFIED.);
#818=B_SPLINE_CURVE_WITH_KNOTS('',3,(#33929,#33930,#33931,#33932,#33933,
#33934,#33935,#33936,#33937,#33938,#33939,#33940,#33941,#33942,#33943,#33944,
#33945,#33946,#33947,#33948,#33949,#33950,#33951,#33952,#33953,#33954,#33955,
#33956,#33957,#33958,#33959,#33960,#33961,#33962,#33963,#33964,#33965,#33966,
#33967,#33968,#33969,#33970,#33971,#33972,#33973,#33974,#33975,#33976,#33977,
#33978,#33979,#33980),.UNSPECIFIED.,.F.,.F.,(4,3,3,3,3,3,3,3,3,3,3,3,3,
3,3,3,3,4),(-0.364629307890686,-0.351116863859227,-0.324664676768481,-0.311283134135643,
-0.274452551481962,-0.262271743112635,-0.225606031128057,-0.200971540009699,
-0.186293214263739,-0.166278288083988,-0.130542983888158,-0.11937084036021,
-0.0895281302701574,-0.0729763635778195,-0.0626462517339964,-0.0518843227274219,
-0.0196324840529713,0.),.UNSPECIFIED.);
#819=B_SPLINE_CURVE_WITH_KNOTS('',3,(#34557,#34558,#34559,#34560,#34561,
#34562,#34563,#34564,#34565,#34566,#34567,#34568,#34569,#34570,#34571,#34572,
#34573,#34574,#34575),.UNSPECIFIED.,.F.,.F.,(4,3,3,3,3,3,4),(133.061082488801,
133.722602823006,134.72053269482,135.718462566633,136.716392438447,137.71432231026,
138.642971792423),.UNSPECIFIED.);
#820=B_SPLINE_CURVE_WITH_KNOTS('',3,(#34577,#34578,#34579,#34580,#34581,
#34582,#34583,#34584,#34585,#34586,#34587,#34588,#34589,#34590,#34591,#34592,
#34593,#34594,#34595,#34596,#34597,#34598,#34599,#34600,#34601,#34602,#34603,
#34604,#34605,#34606,#34607,#34608,#34609,#34610,#34611,#34612,#34613,#34614,
#34615,#34616,#34617,#34618,#34619,#34620,#34621,#34622,#34623,#34624,#34625,
#34626,#34627,#34628),.UNSPECIFIED.,.F.,.F.,(4,3,3,3,3,3,3,3,3,3,3,3,3,
3,3,3,3,4),(-0.366397579005848,-0.355436711127817,-0.328765885668864,-0.316053387324444,
-0.292503977462896,-0.2802316187117,-0.245255597344971,-0.218571154973266,
-0.207922184331738,-0.187195667096965,-0.163796208709844,-0.149553707012105,
-0.138748635975912,-0.104061476981934,-0.0827650184680586,-0.066779980749083,
-0.0282862336556402,0.),.UNSPECIFIED.);
#821=B_SPLINE_CURVE_WITH_KNOTS('',3,(#34629,#34630,#34631,#34632,#34633,
#34634,#34635,#34636,#34637),.UNSPECIFIED.,.F.,.F.,(4,1,1,1,1,1,4),(10.3757270560179,
11.3043765381802,12.3023064099937,13.3002362818072,14.2981661536207,15.2960960254341,
15.7079632679489),.UNSPECIFIED.);
#822=B_SPLINE_CURVE_WITH_KNOTS('',3,(#34643,#34644,#34645,#34646,#34647,
#34648,#34649,#34650,#34651,#34652,#34653,#34654,#34655,#34656,#34657,#34658,
#34659,#34660,#34661,#34662,#34663,#34664,#34665,#34666,#34667,#34668,#34669,
#34670,#34671,#34672,#34673,#34674,#34675,#34676,#34677,#34678,#34679,#34680,
#34681,#34682,#34683,#34684,#34685,#34686,#34687,#34688,#34689,#34690,#34691,
#34692,#34693,#34694),.UNSPECIFIED.,.F.,.F.,(4,3,3,3,3,3,3,3,3,3,3,3,3,
3,3,3,3,4),(-0.364629307890667,-0.351116863859215,-0.324664673225363,-0.311283119253959,
-0.274452522062154,-0.262271701636058,-0.22560598629008,-0.200971428165319,
-0.186293220294034,-0.166278288083978,-0.130542982670707,-0.119370841196389,
-0.0895281308972919,-0.0729763658959894,-0.0626462592378975,-0.0518843246587979,
-0.0196325022123193,0.),.UNSPECIFIED.);
#823=B_SPLINE_CURVE_WITH_KNOTS('',3,(#34697,#34698,#34699,#34700,#34701,
#34702,#34703,#34704),.UNSPECIFIED.,.F.,.F.,(4,1,1,1,1,4),(11.6154215191106,
12.6133513909241,13.6112812627376,14.6092111345511,15.6071410063646,15.7079632679489),
 .UNSPECIFIED.);
#824=B_SPLINE_CURVE_WITH_KNOTS('',3,(#35281,#35282,#35283,#35284,#35285,
#35286,#35287,#35288,#35289,#35290,#35291,#35292,#35293,#35294,#35295,#35296),
 .UNSPECIFIED.,.F.,.F.,(4,3,3,3,3,4),(-140.708111925701,-139.710182053887,
-138.712252182074,-137.71432231026,-136.716392438447,-136.03943319961),
 .UNSPECIFIED.);
#825=B_SPLINE_CURVE_WITH_KNOTS('',3,(#36261,#36262,#36263,#36264,#36265,
#36266,#36267,#36268,#36269,#36270),.UNSPECIFIED.,.F.,.F.,(4,3,3,4),(-4.09254174883833,
-3.97739297481808,-2.98304473111356,-2.06514013327812),.UNSPECIFIED.);
#826=B_SPLINE_CURVE_WITH_KNOTS('',3,(#36273,#36274,#36275,#36276,#36277,
#36278,#36279),.UNSPECIFIED.,.F.,.F.,(4,3,4),(0.,0.994348243704517,1.11419103802957),
 .UNSPECIFIED.);
#827=B_SPLINE_CURVE_WITH_KNOTS('',3,(#36284,#36285,#36286,#36287,#36288,
#36289,#36290,#36291,#36292,#36293,#36294,#36295,#36296,#36297,#36298,#36299,
#36300,#36301,#36302,#36303,#36304,#36305),.UNSPECIFIED.,.F.,.F.,(4,3,3,
3,3,3,3,4),(-10.3757270560179,-9.9434824370452,-8.94913419334068,-7.95478594963616,
-6.96043770593164,-5.96608946222712,-4.9717412185226,-4.09254174883833),
 .UNSPECIFIED.);
#828=B_SPLINE_CURVE_WITH_KNOTS('',3,(#36306,#36307,#36308,#36309,#36310,
#36311,#36312,#36313,#36314,#36315,#36316,#36317,#36318,#36319,#36320,#36321,
#36322,#36323,#36324,#36325,#36326,#36327),.UNSPECIFIED.,.F.,.F.,(4,3,3,
3,3,3,3,4),(1.11419103802957,1.98869648740904,2.98304473111356,3.97739297481808,
4.9717412185226,5.96608946222712,6.96043770593164,7.39737634520915),
 .UNSPECIFIED.);
#829=B_SPLINE_CURVE_WITH_KNOTS('',3,(#36332,#36333,#36334,#36335,#36336,
#36337,#36338,#36339,#36340,#36341,#36342,#36343,#36344,#36345,#36346,#36347,
#36348,#36349,#36350,#36351,#36352,#36353),.UNSPECIFIED.,.F.,.F.,(4,3,3,
3,3,3,3,4),(-16.6589123631975,-15.9095718992723,-14.9152236555678,-13.9208754118633,
-12.9265271681588,-11.9321789244542,-10.9378306807497,-10.3757270560179),
 .UNSPECIFIED.);
#830=B_SPLINE_CURVE_WITH_KNOTS('',3,(#36354,#36355,#36356,#36357,#36358,
#36359,#36360,#36361,#36362,#36363,#36364,#36365,#36366,#36367,#36368,#36369,
#36370,#36371,#36372,#36373,#36374,#36375),.UNSPECIFIED.,.F.,.F.,(4,3,3,
3,3,3,3,4),(7.39737634520915,7.95478594963616,8.94913419334068,9.9434824370452,
10.9378306807497,11.9321789244542,12.9265271681588,13.6805616523887),
 .UNSPECIFIED.);
#831=B_SPLINE_CURVE_WITH_KNOTS('',3,(#36380,#36381,#36382,#36383,#36384,
#36385,#36386,#36387,#36388,#36389,#36390,#36391,#36392,#36393,#36394,#36395,
#36396,#36397,#36398,#36399,#36400,#36401,#36402,#36403,#36404),
 .UNSPECIFIED.,.F.,.F.,(4,3,3,3,3,3,3,3,4),(-22.9420976703771,-22.8700096052039,
-21.8756613614994,-20.8813131177949,-19.8869648740904,-18.8926166303859,
-17.8982683866814,-16.9039201429768,-16.6589123631975),.UNSPECIFIED.);
#832=B_SPLINE_CURVE_WITH_KNOTS('',3,(#36405,#36406,#36407,#36408,#36409,
#36410,#36411,#36412,#36413,#36414,#36415,#36416,#36417,#36418,#36419,#36420,
#36421,#36422,#36423,#36424,#36425,#36426,#36427,#36428,#36429),
 .UNSPECIFIED.,.F.,.F.,(4,3,3,3,3,3,3,3,4),(13.6805616523887,13.9208754118633,
14.9152236555678,15.9095718992723,16.9039201429768,17.8982683866814,18.8926166303859,
19.8869648740904,19.9637469595683),.UNSPECIFIED.);
#833=B_SPLINE_CURVE_WITH_KNOTS('',3,(#36434,#36435,#36436,#36437,#36438,
#36439,#36440,#36441,#36442,#36443,#36444,#36445,#36446,#36447,#36448,#36449,
#36450,#36451,#36452,#36453,#36454,#36455),.UNSPECIFIED.,.F.,.F.,(4,3,3,
3,3,3,3,4),(-29.2252829775567,-28.8360990674311,-27.8417508237265,-26.847402580022,
-25.8530543363175,-24.858706092613,-23.8643578489085,-22.9420976703771),
 .UNSPECIFIED.);
#834=B_SPLINE_CURVE_WITH_KNOTS('',3,(#36456,#36457,#36458,#36459,#36460,
#36461,#36462,#36463,#36464,#36465,#36466,#36467,#36468,#36469,#36470,#36471,
#36472,#36473,#36474,#36475,#36476,#36477),.UNSPECIFIED.,.F.,.F.,(4,3,3,
3,3,3,3,4),(19.9637469595683,20.8813131177949,21.8756613614994,22.8700096052039,
23.8643578489085,24.858706092613,25.8530543363175,26.2469322667479),
 .UNSPECIFIED.);
#835=B_SPLINE_CURVE_WITH_KNOTS('',3,(#36482,#36483,#36484,#36485,#36486,
#36487,#36488,#36489,#36490,#36491,#36492,#36493,#36494,#36495,#36496,#36497,
#36498,#36499,#36500,#36501,#36502,#36503),.UNSPECIFIED.,.F.,.F.,(4,3,3,
3,3,3,3,4),(-35.5084682847363,-34.8021885296582,-33.8078402859537,-32.8134920422491,
-31.8191437985446,-30.8247955548401,-29.8304473111356,-29.2252829775567),
 .UNSPECIFIED.);
#836=B_SPLINE_CURVE_WITH_KNOTS('',3,(#36504,#36505,#36506,#36507,#36508,
#36509,#36510,#36511,#36512,#36513,#36514,#36515,#36516,#36517,#36518,#36519,
#36520,#36521,#36522,#36523,#36524,#36525),.UNSPECIFIED.,.F.,.F.,(4,3,3,
3,3,3,3,4),(26.2469322667479,26.847402580022,27.8417508237265,28.8360990674311,
29.8304473111356,30.8247955548401,31.8191437985446,32.5301175739275),
 .UNSPECIFIED.);
#837=B_SPLINE_CURVE_WITH_KNOTS('',3,(#36530,#36531,#36532,#36533,#36534,
#36535,#36536,#36537,#36538,#36539,#36540,#36541,#36542,#36543,#36544,#36545,
#36546,#36547,#36548,#36549,#36550,#36551,#36552,#36553,#36554),
 .UNSPECIFIED.,.F.,.F.,(4,3,3,3,3,3,3,3,4),(-41.7916535919159,-41.7626262355898,
-40.7682779918853,-39.7739297481808,-38.7795815044762,-37.7852332607717,
-36.7908850170672,-35.7965367733627,-35.5084682847363),.UNSPECIFIED.);
#838=B_SPLINE_CURVE_WITH_KNOTS('',3,(#36555,#36556,#36557,#36558,#36559,
#36560,#36561,#36562,#36563,#36564,#36565,#36566,#36567,#36568,#36569,#36570,
#36571,#36572,#36573,#36574,#36575,#36576,#36577,#36578,#36579),
 .UNSPECIFIED.,.F.,.F.,(4,3,3,3,3,3,3,3,4),(32.5301175739275,32.8134920422491,
33.8078402859537,34.8021885296582,35.7965367733627,36.7908850170672,37.7852332607717,
38.7795815044763,38.8133028811071),.UNSPECIFIED.);
#839=B_SPLINE_CURVE_WITH_KNOTS('',3,(#36584,#36585,#36586,#36587,#36588,
#36589,#36590,#36591,#36592,#36593,#36594,#36595,#36596,#36597,#36598,#36599,
#36600,#36601,#36602,#36603,#36604,#36605),.UNSPECIFIED.,.F.,.F.,(4,3,3,
3,3,3,3,4),(-48.0748388990954,-47.7287156978169,-46.7343674541124,-45.7400192104079,
-44.7456709667034,-43.7513227229988,-42.7569744792943,-41.7916535919159),
 .UNSPECIFIED.);
#840=B_SPLINE_CURVE_WITH_KNOTS('',3,(#36606,#36607,#36608,#36609,#36610,
#36611,#36612,#36613,#36614,#36615,#36616,#36617,#36618,#36619,#36620,#36621,
#36622,#36623,#36624,#36625,#36626,#36627),.UNSPECIFIED.,.F.,.F.,(4,3,3,
3,3,3,3,4),(38.8133028811071,39.7739297481808,40.7682779918853,41.7626262355898,
42.7569744792943,43.7513227229989,44.7456709667034,45.0964881882867),
 .UNSPECIFIED.);
#841=B_SPLINE_CURVE_WITH_KNOTS('',3,(#36632,#36633,#36634,#36635,#36636,
#36637,#36638,#36639,#36640,#36641,#36642,#36643,#36644,#36645,#36646,#36647,
#36648,#36649,#36650,#36651,#36652,#36653),.UNSPECIFIED.,.F.,.F.,(4,3,3,
3,3,3,3,4),(-54.3580242062751,-53.694805160044,-52.7004569163395,-51.706108672635,
-50.7117604289305,-49.717412185226,-48.7230639415214,-48.0748388990954),
 .UNSPECIFIED.);
#842=B_SPLINE_CURVE_WITH_KNOTS('',3,(#36654,#36655,#36656,#36657,#36658,
#36659,#36660,#36661,#36662,#36663,#36664,#36665,#36666,#36667,#36668,#36669,
#36670,#36671,#36672,#36673,#36674,#36675),.UNSPECIFIED.,.F.,.F.,(4,3,3,
3,3,3,3,4),(45.0964881882867,45.7400192104079,46.7343674541124,47.7287156978169,
48.7230639415215,49.717412185226,50.7117604289305,51.3796734954663),
 .UNSPECIFIED.);
#843=B_SPLINE_CURVE_WITH_KNOTS('',3,(#36680,#36681,#36682,#36683,#36684,
#36685,#36686,#36687,#36688,#36689,#36690,#36691,#36692,#36693,#36694,#36695,
#36696,#36697,#36698,#36699,#36700,#36701),.UNSPECIFIED.,.F.,.F.,(4,3,3,
3,3,3,3,4),(-60.6412095134546,-59.6608946222712,-58.6665463785667,-57.6721981348621,
-56.6778498911576,-55.6835016474531,-54.6891534037486,-54.3580242062751),
 .UNSPECIFIED.);
#844=B_SPLINE_CURVE_WITH_KNOTS('',3,(#36702,#36703,#36704,#36705,#36706,
#36707,#36708,#36709,#36710,#36711,#36712,#36713,#36714,#36715,#36716,#36717,
#36718,#36719,#36720,#36721,#36722,#36723),.UNSPECIFIED.,.F.,.F.,(4,3,3,
3,3,3,3,4),(51.3796734954663,51.706108672635,52.7004569163395,53.6948051600441,
54.6891534037486,55.6835016474531,56.6778498911576,57.6628588026459),
 .UNSPECIFIED.);
#845=B_SPLINE_CURVE_WITH_KNOTS('',3,(#36728,#36729,#36730,#36731,#36732,
#36733,#36734,#36735,#36736,#36737,#36738,#36739,#36740,#36741,#36742,#36743,
#36744,#36745,#36746,#36747,#36748,#36749,#36750,#36751,#36752),
 .UNSPECIFIED.,.F.,.F.,(4,3,3,3,3,3,3,3,4),(-66.9243948206342,-66.6213323282028,
-65.6269840844983,-64.6326358407938,-63.6382875970892,-62.6439393533847,
-61.6495911096802,-60.6552428659757,-60.6412095134546),.UNSPECIFIED.);
#846=B_SPLINE_CURVE_WITH_KNOTS('',3,(#36753,#36754,#36755,#36756,#36757,
#36758,#36759,#36760,#36761,#36762,#36763,#36764,#36765,#36766,#36767,#36768,
#36769,#36770,#36771,#36772,#36773,#36774,#36775,#36776,#36777),
 .UNSPECIFIED.,.F.,.F.,(4,3,3,3,3,3,3,3,4),(57.6628588026459,57.6721981348621,
58.6665463785666,59.6608946222712,60.6552428659757,61.6495911096802,62.6439393533847,
63.6382875970892,63.9460441098255),.UNSPECIFIED.);
#847=B_SPLINE_CURVE_WITH_KNOTS('',3,(#36783,#36784,#36785,#36786,#36787,
#36788),.UNSPECIFIED.,.F.,.F.,(4,1,1,4),(78.5398163397449,79.2311020910179,
80.2254503347224,81.1433549325579),.UNSPECIFIED.);
#848=B_SPLINE_CURVE_WITH_KNOTS('',3,(#36791,#36792,#36793,#36794,#36795),
 .UNSPECIFIED.,.F.,.F.,(4,1,4),(78.5398163397448,78.9093122257606,79.9036604694651),
 .UNSPECIFIED.);
#849=B_SPLINE_CURVE_WITH_KNOTS('',3,(#36800,#36801,#36802,#36803,#36804,
#36805,#36806,#36807,#36808,#36809,#36810),.UNSPECIFIED.,.F.,.F.,(4,1,1,
1,1,1,1,1,4),(72.2566310325653,72.2706643850863,73.2650126287908,74.2593608724953,
75.2537091161998,76.2480573599044,77.2424056036089,78.2367538473134,78.5398163397449),
 .UNSPECIFIED.);
#850=B_SPLINE_CURVE_WITH_KNOTS('',3,(#36811,#36812,#36813,#36814,#36815,
#36816,#36817,#36818,#36819,#36820),.UNSPECIFIED.,.F.,.F.,(4,1,1,1,1,1,
1,4),(72.2566310325652,72.9432227635335,73.937571007238,74.9319192509425,
75.926267494647,76.9206157383516,77.9149639820561,78.5398163397448),
 .UNSPECIFIED.);
#851=B_SPLINE_CURVE_WITH_KNOTS('',3,(#36825,#36826,#36827,#36828,#36829,
#36830,#36831,#36832,#36833,#36834),.UNSPECIFIED.,.F.,.F.,(4,1,1,1,1,1,
1,4),(65.9734457253856,66.3045749228592,67.2989231665637,68.2932714102682,
69.2876196539727,70.2819678976772,71.2763161413818,72.2566310325653),
 .UNSPECIFIED.);
#852=B_SPLINE_CURVE_WITH_KNOTS('',3,(#36835,#36836,#36837,#36838,#36839,
#36840,#36841,#36842,#36843,#36844,#36845),.UNSPECIFIED.,.F.,.F.,(4,1,1,
1,1,1,1,1,4),(65.9734457253856,65.9827850576018,66.9771333013064,67.9714815450109,
68.9658297887154,69.9601780324199,70.9545262761244,71.948874519829,72.2566310325652),
 .UNSPECIFIED.);
#853=B_SPLINE_CURVE_WITH_KNOTS('',3,(#36850,#36851,#36852,#36853,#36854,
#36855,#36856,#36857,#36858,#36859),.UNSPECIFIED.,.F.,.F.,(4,1,1,1,1,1,
1,4),(59.6902604182061,60.338485460632,61.3328337043366,62.3271819480411,
63.3215301917456,64.3158784354501,65.3102266791546,65.9734457253856),
 .UNSPECIFIED.);
#854=B_SPLINE_CURVE_WITH_KNOTS('',3,(#36860,#36861,#36862,#36863,#36864,
#36865,#36866,#36867,#36868,#36869),.UNSPECIFIED.,.F.,.F.,(4,1,1,1,1,1,
1,4),(59.6902604182061,60.0166955953747,61.0110438390793,62.0053920827838,
62.9997403264883,63.9940885701928,64.9884368138973,65.9734457253856),
 .UNSPECIFIED.);
#855=B_SPLINE_CURVE_WITH_KNOTS('',3,(#36874,#36875,#36876,#36877,#36878,
#36879,#36880,#36881,#36882,#36883),.UNSPECIFIED.,.F.,.F.,(4,1,1,1,1,1,
1,4),(53.4070751110265,54.3723959984049,55.3667442421094,56.361092485814,
57.3554407295185,58.349788973223,59.3441372169275,59.6902604182061),
 .UNSPECIFIED.);
#856=B_SPLINE_CURVE_WITH_KNOTS('',3,(#36884,#36885,#36886,#36887,#36888,
#36889,#36890,#36891,#36892,#36893),.UNSPECIFIED.,.F.,.F.,(4,1,1,1,1,1,
1,4),(53.4070751110265,54.0506061331476,55.0449543768521,56.0393026205567,
57.0336508642612,58.0279991079657,59.0223473516702,59.6902604182061),
 .UNSPECIFIED.);
#857=B_SPLINE_CURVE_WITH_KNOTS('',3,(#36898,#36899,#36900,#36901,#36902,
#36903,#36904,#36905,#36906,#36907,#36908),.UNSPECIFIED.,.F.,.F.,(4,1,1,
1,1,1,1,1,4),(47.1238898038469,47.4119582924733,48.4063065361778,49.4006547798823,
50.3950030235868,51.3893512672914,52.3836995109959,53.3780477547004,53.4070751110265),
 .UNSPECIFIED.);
#858=B_SPLINE_CURVE_WITH_KNOTS('',3,(#36909,#36910,#36911,#36912,#36913,
#36914,#36915,#36916,#36917,#36918),.UNSPECIFIED.,.F.,.F.,(4,1,1,1,1,1,
1,4),(47.1238898038469,48.0845166709205,49.078864914625,50.0732131583295,
51.0675614020341,52.0619096457386,53.0562578894431,53.4070751110265),
 .UNSPECIFIED.);
#859=B_SPLINE_CURVE_WITH_KNOTS('',3,(#36923,#36924,#36925,#36926,#36927,
#36928,#36929,#36930,#36931,#36932),.UNSPECIFIED.,.F.,.F.,(4,1,1,1,1,1,
1,4),(40.8407044966673,41.4458688302462,42.4402170739507,43.4345653176552,
44.4289135613597,45.4232618050643,46.4176100487688,47.1238898038469),
 .UNSPECIFIED.);
#860=B_SPLINE_CURVE_WITH_KNOTS('',3,(#36933,#36934,#36935,#36936,#36937,
#36938,#36939,#36940,#36941,#36942,#36943),.UNSPECIFIED.,.F.,.F.,(4,1,1,
1,1,1,1,1,4),(40.8407044966673,41.1240789649889,42.1184272086934,43.1127754523979,
44.1071236961024,45.1014719398069,46.0958201835115,47.090168427216,47.1238898038469),
 .UNSPECIFIED.);
#861=B_SPLINE_CURVE_WITH_KNOTS('',3,(#36948,#36949,#36950,#36951,#36952,
#36953,#36954,#36955,#36956,#36957),.UNSPECIFIED.,.F.,.F.,(4,1,1,1,1,1,
1,4),(34.5575191894877,35.4797793680191,36.4741276117236,37.4684758554281,
38.4628240991326,39.4571723428371,40.4515205865417,40.8407044966673),
 .UNSPECIFIED.);
#862=B_SPLINE_CURVE_WITH_KNOTS('',3,(#36958,#36959,#36960,#36961,#36962,
#36963,#36964,#36965,#36966,#36967),.UNSPECIFIED.,.F.,.F.,(4,1,1,1,1,1,
1,4),(34.5575191894877,35.1579895027618,36.1523377464663,37.1466859901708,
38.1410342338753,39.1353824775798,40.1297307212843,40.8407044966673),
 .UNSPECIFIED.);
#863=B_SPLINE_CURVE_WITH_KNOTS('',3,(#36972,#36973,#36974,#36975,#36976,
#36977,#36978,#36979,#36980,#36981,#36982),.UNSPECIFIED.,.F.,.F.,(4,1,1,
1,1,1,1,1,4),(28.2743338823081,28.5193416620874,29.5136899057919,30.5080381494965,
31.502386393201,32.4967346369055,33.49108288061,34.4854311243145,34.5575191894877),
 .UNSPECIFIED.);
#864=B_SPLINE_CURVE_WITH_KNOTS('',3,(#36983,#36984,#36985,#36986,#36987,
#36988,#36989,#36990,#36991,#36992),.UNSPECIFIED.,.F.,.F.,(4,1,1,1,1,1,
1,4),(28.2743338823081,29.1919000405346,30.1862482842392,31.1805965279437,
32.1749447716482,33.1692930153527,34.1636412590572,34.5575191894877),
 .UNSPECIFIED.);
#865=B_SPLINE_CURVE_WITH_KNOTS('',3,(#36997,#36998,#36999,#37000,#37001,
#37002,#37003,#37004,#37005,#37006),.UNSPECIFIED.,.F.,.F.,(4,1,1,1,1,1,
1,4),(21.9911485751285,22.5532521998603,23.5476004435648,24.5419486872693,
25.5362969309739,26.5306451746784,27.5249934183829,28.2743338823081),
 .UNSPECIFIED.);
#866=B_SPLINE_CURVE_WITH_KNOTS('',3,(#37007,#37008,#37009,#37010,#37011,
#37012,#37013,#37014,#37015,#37016,#37017),.UNSPECIFIED.,.F.,.F.,(4,1,1,
1,1,1,1,1,4),(21.9911485751285,22.231462334603,23.2258105783075,24.220158822012,
25.2145070657166,26.2088553094211,27.2032035531256,28.1975517968301,28.2743338823081),
 .UNSPECIFIED.);
#867=B_SPLINE_CURVE_WITH_KNOTS('',3,(#37022,#37023,#37024,#37025,#37026,
#37027,#37028,#37029,#37030,#37031),.UNSPECIFIED.,.F.,.F.,(4,1,1,1,1,1,
1,4),(15.7079632679489,16.5871627376332,17.5815109813377,18.5758592250422,
19.5702074687467,20.5645557124513,21.5589039561558,21.9911485751285),
 .UNSPECIFIED.);
#868=B_SPLINE_CURVE_WITH_KNOTS('',3,(#37032,#37033,#37034,#37035,#37036,
#37037,#37038,#37039,#37040,#37041),.UNSPECIFIED.,.F.,.F.,(4,1,1,1,1,1,
1,4),(15.7079632679489,16.2653728723759,17.2597211160804,18.2540693597849,
19.2484176034894,20.242765847194,21.2371140908985,21.9911485751285),
 .UNSPECIFIED.);
#869=B_SPLINE_CURVE_WITH_KNOTS('',3,(#37343,#37344,#37345,#37346,#37347,
#37348,#37349,#37350,#37351,#37352,#37353,#37354,#37355,#37356,#37357,#37358,
#37359,#37360,#37361,#37362,#37363,#37364,#37365,#37366,#37367,#37368,#37369,
#37370,#37371,#37372,#37373,#37374,#37375,#37376,#37377,#37378,#37379,#37380,
#37381,#37382,#37383,#37384,#37385,#37386,#37387,#37388,#37389,#37390,#37391,
#37392,#37393,#37394,#37395,#37396,#37397),.UNSPECIFIED.,.F.,.F.,(4,3,3,
3,3,3,3,3,3,3,3,3,3,3,3,3,3,3,4),(-0.364629307890675,-0.34972378827242,
-0.322720263625586,-0.304347638378591,-0.283123644987568,-0.264601682105285,
-0.252328648782195,-0.215920039519477,-0.197925115950283,-0.186636791761712,
-0.165647166431853,-0.140760913934002,-0.127055807624798,-0.116187295826016,
-0.0871404718695121,-0.0682560541634265,-0.0546745507926151,-0.0223452933345784,
0.),.UNSPECIFIED.);
#870=B_SPLINE_CURVE_WITH_KNOTS('',3,(#37398,#37399,#37400,#37401,#37402,
#37403,#37404,#37405,#37406,#37407,#37408,#37409,#37410,#37411,#37412,#37413,
#37414,#37415,#37416),.UNSPECIFIED.,.F.,.F.,(4,3,3,3,3,3,4),(63.9460441098255,
64.6326358407938,65.6269840844983,66.6213323282028,67.6156805719073,68.6100288156118,
69.5279334134473),.UNSPECIFIED.);
#871=B_SPLINE_CURVE_WITH_KNOTS('',3,(#37418,#37419,#37420,#37421,#37422,
#37423,#37424,#37425,#37426,#37427,#37428,#37429,#37430,#37431,#37432,#37433,
#37434,#37435,#37436,#37437,#37438,#37439,#37440,#37441,#37442,#37443,#37444,
#37445,#37446,#37447,#37448,#37449,#37450,#37451,#37452,#37453,#37454,#37455,
#37456,#37457,#37458,#37459,#37460,#37461,#37462,#37463,#37464,#37465,#37466,
#37467,#37468,#37469),.UNSPECIFIED.,.F.,.F.,(4,3,3,3,3,3,3,3,3,3,3,3,3,
3,3,3,3,4),(-0.366397579005845,-0.354297286130077,-0.32692051483854,-0.315737482103616,
-0.289774380161196,-0.272943837084162,-0.237814929253474,-0.221139930607587,
-0.207673366759947,-0.18655652524636,-0.163236959590565,-0.1482203546737,
-0.138085786201687,-0.103564339651265,-0.0816322651568354,-0.0668657996484716,
-0.0283713742630058,0.),.UNSPECIFIED.);
#872=B_SPLINE_CURVE_WITH_KNOTS('',3,(#37470,#37471,#37472,#37473,#37474,
#37475,#37476,#37477,#37478),.UNSPECIFIED.,.F.,.F.,(4,1,1,1,1,1,4),(10.3757270560178,
11.2936316538533,12.2879798975578,13.2823281412623,14.2766763849668,15.2710246286714,
15.7079632679489),.UNSPECIFIED.);
#873=B_SPLINE_CURVE_WITH_KNOTS('',3,(#37484,#37485,#37486,#37487,#37488,
#37489,#37490,#37491,#37492,#37493,#37494,#37495,#37496,#37497,#37498,#37499,
#37500,#37501,#37502,#37503,#37504,#37505,#37506,#37507,#37508,#37509,#37510,
#37511,#37512,#37513,#37514,#37515,#37516,#37517,#37518,#37519,#37520,#37521,
#37522,#37523,#37524,#37525,#37526,#37527,#37528,#37529,#37530,#37531,#37532,
#37533,#37534,#37535,#37536,#37537,#37538),.UNSPECIFIED.,.F.,.F.,(4,3,3,
3,3,3,3,3,3,3,3,3,3,3,3,3,3,3,4),(-0.364629307890664,-0.349723788272418,
-0.32272025631553,-0.304347635918125,-0.283123621269396,-0.264601511160708,
-0.252328600826691,-0.2159199799845,-0.197925046601542,-0.186636790019817,
-0.165647166431849,-0.140761503006746,-0.127058155986358,-0.116187684714683,
-0.0871407635360122,-0.0682567232080817,-0.0546745590404074,-0.0223453321529391,
0.),.UNSPECIFIED.);
#874=B_SPLINE_CURVE_WITH_KNOTS('',3,(#37541,#37542,#37543,#37544,#37545,
#37546,#37547,#37548),.UNSPECIFIED.,.F.,.F.,(4,1,1,1,1,4),(11.6154215191106,
12.6097697628151,13.6041180065196,14.5984662502242,15.5928144939287,15.7079632679489),
 .UNSPECIFIED.);
#875=B_SPLINE_CURVE_WITH_KNOTS('',3,(#37850,#37851,#37852,#37853,#37854,
#37855,#37856,#37857,#37858,#37859,#37860,#37861,#37862,#37863,#37864,#37865,
#37866,#37867,#37868,#37869,#37870,#37871,#37872,#37873,#37874,#37875,#37876,
#37877,#37878,#37879,#37880,#37881,#37882,#37883,#37884,#37885,#37886,#37887,
#37888,#37889,#37890,#37891,#37892,#37893,#37894,#37895,#37896,#37897,#37898,
#37899,#37900,#37901),.UNSPECIFIED.,.F.,.F.,(4,3,3,3,3,3,3,3,3,3,3,3,3,
3,3,3,3,4),(-0.366397579005866,-0.354297286130098,-0.326920513926121,-0.315737475841804,
-0.28977472454701,-0.272943757381991,-0.237814845664656,-0.221139815084396,
-0.207673346380608,-0.186556525246364,-0.163236959590568,-0.148220372021337,
-0.138085817027126,-0.103564362770345,-0.0816323215052509,-0.0668658025503337,
-0.0283713861783979,0.),.UNSPECIFIED.);
#876=B_SPLINE_CURVE_WITH_KNOTS('',3,(#37902,#37903,#37904,#37905,#37906,
#37907,#37908,#37909,#37910,#37911,#37912,#37913,#37914,#37915,#37916,#37917),
 .UNSPECIFIED.,.F.,.F.,(4,3,3,3,3,4),(-71.5930735467254,-70.5987253030209,
-69.6043770593164,-68.6100288156118,-67.6156805719073,-66.9243948206342),
 .UNSPECIFIED.);
#877=CYLINDRICAL_SURFACE('',#16433,1.);
#878=CYLINDRICAL_SURFACE('',#16435,0.205);
#879=CYLINDRICAL_SURFACE('',#16453,0.4);
#880=CYLINDRICAL_SURFACE('',#16456,0.4);
#881=CYLINDRICAL_SURFACE('',#16506,1.6);
#882=CYLINDRICAL_SURFACE('',#16551,0.325);
#883=CYLINDRICAL_SURFACE('',#16555,0.325);
#884=CYLINDRICAL_SURFACE('',#16573,0.4);
#885=CYLINDRICAL_SURFACE('',#16575,0.4);
#886=CYLINDRICAL_SURFACE('',#16577,0.325);
#887=CYLINDRICAL_SURFACE('',#16580,0.325);
#888=CYLINDRICAL_SURFACE('',#16587,0.205);
#889=CYLINDRICAL_SURFACE('',#16595,0.205);
#890=CYLINDRICAL_SURFACE('',#16598,0.205);
#891=CYLINDRICAL_SURFACE('',#16601,0.205);
#892=CYLINDRICAL_SURFACE('',#16608,1.);
#893=CYLINDRICAL_SURFACE('',#16614,1.3);
#894=CYLINDRICAL_SURFACE('',#16622,0.705);
#895=CYLINDRICAL_SURFACE('',#16637,0.7);
#896=CYLINDRICAL_SURFACE('',#16701,1.1);
#897=CYLINDRICAL_SURFACE('',#16716,1.26);
#898=CYLINDRICAL_SURFACE('',#16719,1.355);
#899=CYLINDRICAL_SURFACE('',#16722,0.225);
#900=CYLINDRICAL_SURFACE('',#16731,0.225000000000001);
#901=CYLINDRICAL_SURFACE('',#16740,0.255);
#902=CYLINDRICAL_SURFACE('',#16744,0.255000000000001);
#903=CYLINDRICAL_SURFACE('',#16748,0.255);
#904=CYLINDRICAL_SURFACE('',#16759,0.4);
#905=CYLINDRICAL_SURFACE('',#16762,0.4);
#906=CYLINDRICAL_SURFACE('',#16779,1.25);
#907=CYLINDRICAL_SURFACE('',#16785,1.3442);
#908=CYLINDRICAL_SURFACE('',#16786,1.3442);
#909=CYLINDRICAL_SURFACE('',#16787,1.286875);
#910=CYLINDRICAL_SURFACE('',#16789,1.286875);
#911=CYLINDRICAL_SURFACE('',#16798,1.286875);
#912=CYLINDRICAL_SURFACE('',#16800,1.286875);
#913=CYLINDRICAL_SURFACE('',#16806,1.3442);
#914=CYLINDRICAL_SURFACE('',#16808,1.3442);
#915=CYLINDRICAL_SURFACE('',#16817,1.05);
#916=CYLINDRICAL_SURFACE('',#16835,0.1954);
#917=CYLINDRICAL_SURFACE('',#16837,0.1954);
#918=CYLINDRICAL_SURFACE('',#16838,0.1954);
#919=CYLINDRICAL_SURFACE('',#16839,0.1954);
#920=CYLINDRICAL_SURFACE('',#16840,0.1954);
#921=CYLINDRICAL_SURFACE('',#16841,0.1954);
#922=CYLINDRICAL_SURFACE('',#16842,0.15555);
#923=CYLINDRICAL_SURFACE('',#16844,0.15555);
#924=CYLINDRICAL_SURFACE('',#16845,0.15555);
#925=CYLINDRICAL_SURFACE('',#16846,0.15555);
#926=CYLINDRICAL_SURFACE('',#16847,0.15555);
#927=CYLINDRICAL_SURFACE('',#16848,0.15555);
#928=CYLINDRICAL_SURFACE('',#16856,0.15555);
#929=CYLINDRICAL_SURFACE('',#16904,0.1954);
#930=CYLINDRICAL_SURFACE('',#16910,0.1954);
#931=CYLINDRICAL_SURFACE('',#16912,0.1954);
#932=CYLINDRICAL_SURFACE('',#16913,0.1954);
#933=CYLINDRICAL_SURFACE('',#16914,0.1954);
#934=CYLINDRICAL_SURFACE('',#16915,0.1954);
#935=CYLINDRICAL_SURFACE('',#16916,0.15555);
#936=CYLINDRICAL_SURFACE('',#16918,0.15555);
#937=CYLINDRICAL_SURFACE('',#16920,0.15555);
#938=CYLINDRICAL_SURFACE('',#16921,0.15555);
#939=CYLINDRICAL_SURFACE('',#16922,0.15555);
#940=CYLINDRICAL_SURFACE('',#16930,0.15555);
#941=CYLINDRICAL_SURFACE('',#16978,0.1954);
#942=CYLINDRICAL_SURFACE('',#16994,1.2);
#943=CYLINDRICAL_SURFACE('',#16999,0.204999999999999);
#944=CYLINDRICAL_SURFACE('',#17006,0.7);
#945=CYLINDRICAL_SURFACE('',#17051,0.205);
#946=CYLINDRICAL_SURFACE('',#17055,0.205);
#947=CYLINDRICAL_SURFACE('',#17081,1.5);
#948=CYLINDRICAL_SURFACE('',#17097,0.1);
#949=CYLINDRICAL_SURFACE('',#17099,0.24635);
#950=CYLINDRICAL_SURFACE('',#17101,0.24635);
#951=CYLINDRICAL_SURFACE('',#17102,0.24635);
#952=CYLINDRICAL_SURFACE('',#17103,0.24635);
#953=CYLINDRICAL_SURFACE('',#17104,0.24635);
#954=CYLINDRICAL_SURFACE('',#17105,0.24635);
#955=CYLINDRICAL_SURFACE('',#17106,0.24635);
#956=CYLINDRICAL_SURFACE('',#17107,0.24635);
#957=CYLINDRICAL_SURFACE('',#17108,0.24635);
#958=CYLINDRICAL_SURFACE('',#17109,0.24635);
#959=CYLINDRICAL_SURFACE('',#17110,0.24635);
#960=CYLINDRICAL_SURFACE('',#17111,0.24635);
#961=CYLINDRICAL_SURFACE('',#17112,0.24635);
#962=CYLINDRICAL_SURFACE('',#17113,0.24635);
#963=CYLINDRICAL_SURFACE('',#17114,0.24635);
#964=CYLINDRICAL_SURFACE('',#17115,0.24635);
#965=CYLINDRICAL_SURFACE('',#17116,0.24635);
#966=CYLINDRICAL_SURFACE('',#17117,0.24635);
#967=CYLINDRICAL_SURFACE('',#17118,0.24635);
#968=CYLINDRICAL_SURFACE('',#17119,0.24635);
#969=CYLINDRICAL_SURFACE('',#17120,0.24635);
#970=CYLINDRICAL_SURFACE('',#17121,0.24635);
#971=CYLINDRICAL_SURFACE('',#17122,0.24635);
#972=CYLINDRICAL_SURFACE('',#17123,0.24635);
#973=CYLINDRICAL_SURFACE('',#17125,0.217775);
#974=CYLINDRICAL_SURFACE('',#17127,0.217775);
#975=CYLINDRICAL_SURFACE('',#17128,0.217775);
#976=CYLINDRICAL_SURFACE('',#17129,0.217775);
#977=CYLINDRICAL_SURFACE('',#17130,0.217775);
#978=CYLINDRICAL_SURFACE('',#17131,0.217775);
#979=CYLINDRICAL_SURFACE('',#17132,0.217775);
#980=CYLINDRICAL_SURFACE('',#17133,0.217775);
#981=CYLINDRICAL_SURFACE('',#17134,0.217775);
#982=CYLINDRICAL_SURFACE('',#17135,0.217775);
#983=CYLINDRICAL_SURFACE('',#17136,0.217775);
#984=CYLINDRICAL_SURFACE('',#17137,0.217775);
#985=CYLINDRICAL_SURFACE('',#17138,0.217775);
#986=CYLINDRICAL_SURFACE('',#17139,0.217775);
#987=CYLINDRICAL_SURFACE('',#17140,0.217775);
#988=CYLINDRICAL_SURFACE('',#17141,0.217775);
#989=CYLINDRICAL_SURFACE('',#17142,0.217775);
#990=CYLINDRICAL_SURFACE('',#17143,0.217775);
#991=CYLINDRICAL_SURFACE('',#17144,0.217775);
#992=CYLINDRICAL_SURFACE('',#17145,0.217775);
#993=CYLINDRICAL_SURFACE('',#17146,0.217775);
#994=CYLINDRICAL_SURFACE('',#17147,0.217775);
#995=CYLINDRICAL_SURFACE('',#17148,0.217775);
#996=CYLINDRICAL_SURFACE('',#17154,0.151);
#997=CYLINDRICAL_SURFACE('',#17162,0.217775);
#998=CYLINDRICAL_SURFACE('',#17223,0.5);
#999=CYLINDRICAL_SURFACE('',#17226,0.5);
#1000=CYLINDRICAL_SURFACE('',#17229,0.5);
#1001=CYLINDRICAL_SURFACE('',#17232,0.5);
#1002=CYLINDRICAL_SURFACE('',#17235,0.5);
#1003=CYLINDRICAL_SURFACE('',#17238,0.5);
#1004=CYLINDRICAL_SURFACE('',#17241,0.5);
#1005=CYLINDRICAL_SURFACE('',#17244,0.5);
#1006=CYLINDRICAL_SURFACE('',#17247,0.5);
#1007=CYLINDRICAL_SURFACE('',#17250,0.5);
#1008=CYLINDRICAL_SURFACE('',#17253,0.5);
#1009=CYLINDRICAL_SURFACE('',#17256,0.5);
#1010=CYLINDRICAL_SURFACE('',#17259,0.5);
#1011=CYLINDRICAL_SURFACE('',#17262,0.5);
#1012=CYLINDRICAL_SURFACE('',#17265,0.5);
#1013=CYLINDRICAL_SURFACE('',#17268,0.5);
#1014=CYLINDRICAL_SURFACE('',#17271,0.5);
#1015=CYLINDRICAL_SURFACE('',#17274,0.5);
#1016=CYLINDRICAL_SURFACE('',#17277,0.5);
#1017=CYLINDRICAL_SURFACE('',#17280,0.5);
#1018=CYLINDRICAL_SURFACE('',#17283,0.5);
#1019=CYLINDRICAL_SURFACE('',#17286,0.5);
#1020=CYLINDRICAL_SURFACE('',#17289,0.5);
#1021=CYLINDRICAL_SURFACE('',#17292,0.5);
#1022=CYLINDRICAL_SURFACE('',#17295,0.5);
#1023=CYLINDRICAL_SURFACE('',#17298,0.5);
#1024=CYLINDRICAL_SURFACE('',#17301,0.5);
#1025=CYLINDRICAL_SURFACE('',#17304,0.5);
#1026=CYLINDRICAL_SURFACE('',#17307,0.5);
#1027=CYLINDRICAL_SURFACE('',#17310,0.5);
#1028=CYLINDRICAL_SURFACE('',#17318,0.24635);
#1029=CYLINDRICAL_SURFACE('',#17333,0.1954);
#1030=CYLINDRICAL_SURFACE('',#17335,0.1954);
#1031=CYLINDRICAL_SURFACE('',#17336,0.1954);
#1032=CYLINDRICAL_SURFACE('',#17337,0.1954);
#1033=CYLINDRICAL_SURFACE('',#17338,0.1954);
#1034=CYLINDRICAL_SURFACE('',#17339,0.1954);
#1035=CYLINDRICAL_SURFACE('',#17340,0.1954);
#1036=CYLINDRICAL_SURFACE('',#17341,0.1954);
#1037=CYLINDRICAL_SURFACE('',#17342,0.1954);
#1038=CYLINDRICAL_SURFACE('',#17343,0.1954);
#1039=CYLINDRICAL_SURFACE('',#17344,0.1954);
#1040=CYLINDRICAL_SURFACE('',#17345,0.1954);
#1041=CYLINDRICAL_SURFACE('',#17346,0.1954);
#1042=CYLINDRICAL_SURFACE('',#17347,0.1954);
#1043=CYLINDRICAL_SURFACE('',#17348,0.1954);
#1044=CYLINDRICAL_SURFACE('',#17349,0.1954);
#1045=CYLINDRICAL_SURFACE('',#17350,0.1954);
#1046=CYLINDRICAL_SURFACE('',#17351,0.1954);
#1047=CYLINDRICAL_SURFACE('',#17352,0.1954);
#1048=CYLINDRICAL_SURFACE('',#17353,0.1954);
#1049=CYLINDRICAL_SURFACE('',#17354,0.1954);
#1050=CYLINDRICAL_SURFACE('',#17355,0.1954);
#1051=CYLINDRICAL_SURFACE('',#17356,0.15555);
#1052=CYLINDRICAL_SURFACE('',#17358,0.15555);
#1053=CYLINDRICAL_SURFACE('',#17359,0.15555);
#1054=CYLINDRICAL_SURFACE('',#17360,0.15555);
#1055=CYLINDRICAL_SURFACE('',#17361,0.15555);
#1056=CYLINDRICAL_SURFACE('',#17362,0.15555);
#1057=CYLINDRICAL_SURFACE('',#17363,0.15555);
#1058=CYLINDRICAL_SURFACE('',#17364,0.15555);
#1059=CYLINDRICAL_SURFACE('',#17365,0.15555);
#1060=CYLINDRICAL_SURFACE('',#17366,0.15555);
#1061=CYLINDRICAL_SURFACE('',#17367,0.15555);
#1062=CYLINDRICAL_SURFACE('',#17368,0.15555);
#1063=CYLINDRICAL_SURFACE('',#17369,0.15555);
#1064=CYLINDRICAL_SURFACE('',#17370,0.15555);
#1065=CYLINDRICAL_SURFACE('',#17371,0.15555);
#1066=CYLINDRICAL_SURFACE('',#17372,0.15555);
#1067=CYLINDRICAL_SURFACE('',#17373,0.15555);
#1068=CYLINDRICAL_SURFACE('',#17374,0.15555);
#1069=CYLINDRICAL_SURFACE('',#17375,0.15555);
#1070=CYLINDRICAL_SURFACE('',#17376,0.15555);
#1071=CYLINDRICAL_SURFACE('',#17377,0.15555);
#1072=CYLINDRICAL_SURFACE('',#17378,0.15555);
#1073=CYLINDRICAL_SURFACE('',#17386,0.15555);
#1074=CYLINDRICAL_SURFACE('',#17391,0.1954);
#1075=CYLINDRICAL_SURFACE('',#17545,0.35);
#1076=CYLINDRICAL_SURFACE('',#17547,0.35);
#1077=CYLINDRICAL_SURFACE('',#17549,0.35);
#1078=CYLINDRICAL_SURFACE('',#17551,0.35);
#1079=CYLINDRICAL_SURFACE('',#17553,0.35);
#1080=CYLINDRICAL_SURFACE('',#17555,0.35);
#1081=CYLINDRICAL_SURFACE('',#17557,0.35);
#1082=CYLINDRICAL_SURFACE('',#17559,0.35);
#1083=CYLINDRICAL_SURFACE('',#17561,0.35);
#1084=CYLINDRICAL_SURFACE('',#17563,0.35);
#1085=CYLINDRICAL_SURFACE('',#17565,0.35);
#1086=CYLINDRICAL_SURFACE('',#17567,0.35);
#1087=CYLINDRICAL_SURFACE('',#17569,0.35);
#1088=CYLINDRICAL_SURFACE('',#17571,0.35);
#1089=CYLINDRICAL_SURFACE('',#17573,0.35);
#1090=CYLINDRICAL_SURFACE('',#17575,0.35);
#1091=CYLINDRICAL_SURFACE('',#17577,0.35);
#1092=CYLINDRICAL_SURFACE('',#17579,0.35);
#1093=CYLINDRICAL_SURFACE('',#17581,0.35);
#1094=CYLINDRICAL_SURFACE('',#17583,0.35);
#1095=CYLINDRICAL_SURFACE('',#17585,0.35);
#1096=CYLINDRICAL_SURFACE('',#17587,0.35);
#1097=CYLINDRICAL_SURFACE('',#17589,0.35);
#1098=CYLINDRICAL_SURFACE('',#17591,0.35);
#1099=CYLINDRICAL_SURFACE('',#17593,0.35);
#1100=CYLINDRICAL_SURFACE('',#17595,0.35);
#1101=CYLINDRICAL_SURFACE('',#17597,0.35);
#1102=CYLINDRICAL_SURFACE('',#17599,0.35);
#1103=CYLINDRICAL_SURFACE('',#17601,0.35);
#1104=CYLINDRICAL_SURFACE('',#17603,0.35);
#1105=CYLINDRICAL_SURFACE('',#17605,0.35);
#1106=CYLINDRICAL_SURFACE('',#17607,0.35);
#1107=CYLINDRICAL_SURFACE('',#17609,0.35);
#1108=CYLINDRICAL_SURFACE('',#17611,0.35);
#1109=CYLINDRICAL_SURFACE('',#17613,0.35);
#1110=CYLINDRICAL_SURFACE('',#17615,0.35);
#1111=CYLINDRICAL_SURFACE('',#17624,0.1954);
#1112=CYLINDRICAL_SURFACE('',#17626,0.1954);
#1113=CYLINDRICAL_SURFACE('',#17627,0.1954);
#1114=CYLINDRICAL_SURFACE('',#17628,0.1954);
#1115=CYLINDRICAL_SURFACE('',#17629,0.1954);
#1116=CYLINDRICAL_SURFACE('',#17630,0.1954);
#1117=CYLINDRICAL_SURFACE('',#17631,0.1954);
#1118=CYLINDRICAL_SURFACE('',#17632,0.1954);
#1119=CYLINDRICAL_SURFACE('',#17633,0.1954);
#1120=CYLINDRICAL_SURFACE('',#17634,0.1954);
#1121=CYLINDRICAL_SURFACE('',#17635,0.1954);
#1122=CYLINDRICAL_SURFACE('',#17636,0.15555);
#1123=CYLINDRICAL_SURFACE('',#17638,0.15555);
#1124=CYLINDRICAL_SURFACE('',#17639,0.15555);
#1125=CYLINDRICAL_SURFACE('',#17640,0.15555);
#1126=CYLINDRICAL_SURFACE('',#17641,0.15555);
#1127=CYLINDRICAL_SURFACE('',#17642,0.15555);
#1128=CYLINDRICAL_SURFACE('',#17643,0.15555);
#1129=CYLINDRICAL_SURFACE('',#17644,0.15555);
#1130=CYLINDRICAL_SURFACE('',#17645,0.15555);
#1131=CYLINDRICAL_SURFACE('',#17646,0.15555);
#1132=CYLINDRICAL_SURFACE('',#17647,0.15555);
#1133=CYLINDRICAL_SURFACE('',#17652,0.15555);
#1134=CYLINDRICAL_SURFACE('',#17701,0.4);
#1135=CYLINDRICAL_SURFACE('',#17704,0.4);
#1136=CYLINDRICAL_SURFACE('',#17707,0.4);
#1137=CYLINDRICAL_SURFACE('',#17710,0.4);
#1138=CYLINDRICAL_SURFACE('',#17713,0.4);
#1139=CYLINDRICAL_SURFACE('',#17716,0.4);
#1140=CYLINDRICAL_SURFACE('',#17719,0.4);
#1141=CYLINDRICAL_SURFACE('',#17722,0.4);
#1142=CYLINDRICAL_SURFACE('',#17725,0.4);
#1143=CYLINDRICAL_SURFACE('',#17728,0.4);
#1144=CYLINDRICAL_SURFACE('',#17731,0.4);
#1145=CYLINDRICAL_SURFACE('',#17734,0.4);
#1146=CYLINDRICAL_SURFACE('',#17737,0.4);
#1147=CYLINDRICAL_SURFACE('',#17740,0.4);
#1148=CYLINDRICAL_SURFACE('',#17743,0.4);
#1149=CYLINDRICAL_SURFACE('',#17746,0.4);
#1150=CYLINDRICAL_SURFACE('',#17749,0.4);
#1151=CYLINDRICAL_SURFACE('',#17752,0.4);
#1152=CYLINDRICAL_SURFACE('',#17755,0.4);
#1153=CYLINDRICAL_SURFACE('',#17758,0.4);
#1154=CYLINDRICAL_SURFACE('',#17761,0.4);
#1155=CYLINDRICAL_SURFACE('',#17764,0.4);
#1156=CYLINDRICAL_SURFACE('',#17767,0.4);
#1157=CYLINDRICAL_SURFACE('',#17770,0.4);
#1158=CYLINDRICAL_SURFACE('',#17778,0.1954);
#1159=FACE_BOUND('',#2713,.T.);
#1160=FACE_BOUND('',#2716,.T.);
#1161=FACE_BOUND('',#2766,.T.);
#1162=FACE_BOUND('',#2769,.T.);
#1163=FACE_BOUND('',#2820,.T.);
#1164=FACE_BOUND('',#2825,.T.);
#1165=FACE_BOUND('',#2837,.T.);
#1166=FACE_BOUND('',#2840,.T.);
#1167=FACE_BOUND('',#2843,.T.);
#1168=FACE_BOUND('',#2846,.T.);
#1169=FACE_BOUND('',#2892,.T.);
#1170=FACE_BOUND('',#2893,.T.);
#1171=FACE_BOUND('',#2894,.T.);
#1172=FACE_BOUND('',#2895,.T.);
#1173=FACE_BOUND('',#2896,.T.);
#1174=FACE_BOUND('',#2897,.T.);
#1175=FACE_BOUND('',#2908,.T.);
#1176=FACE_BOUND('',#2911,.T.);
#1177=FACE_BOUND('',#2919,.T.);
#1178=FACE_BOUND('',#2924,.T.);
#1179=FACE_BOUND('',#2933,.T.);
#1180=FACE_BOUND('',#2934,.T.);
#1181=FACE_BOUND('',#2935,.T.);
#1182=FACE_BOUND('',#2936,.T.);
#1183=FACE_BOUND('',#2937,.T.);
#1184=FACE_BOUND('',#2938,.T.);
#1185=FACE_BOUND('',#2990,.T.);
#1186=FACE_BOUND('',#3044,.T.);
#1187=FACE_BOUND('',#3096,.T.);
#1188=FACE_BOUND('',#3107,.T.);
#1189=FACE_BOUND('',#3114,.T.);
#1190=FACE_BOUND('',#3117,.T.);
#1191=FACE_BOUND('',#3146,.T.);
#1192=FACE_BOUND('',#3147,.T.);
#1193=FACE_BOUND('',#3148,.T.);
#1194=FACE_BOUND('',#3149,.T.);
#1195=FACE_BOUND('',#3150,.T.);
#1196=FACE_BOUND('',#3165,.T.);
#1197=FACE_BOUND('',#3166,.T.);
#1198=FACE_BOUND('',#3167,.T.);
#1199=FACE_BOUND('',#3339,.T.);
#1200=FACE_BOUND('',#3343,.T.);
#1201=FACE_BOUND('',#3346,.T.);
#1202=FACE_BOUND('',#3403,.T.);
#1203=FACE_BOUND('',#3547,.T.);
#1204=FACE_BOUND('',#3651,.T.);
#1205=CIRCLE('',#16425,1.0287867965644);
#1206=CIRCLE('',#16426,1.08);
#1207=CIRCLE('',#16428,1.0212132034356);
#1208=CIRCLE('',#16430,1.54);
#1209=CIRCLE('',#16432,1.);
#1210=CIRCLE('',#16434,1.);
#1211=CIRCLE('',#16445,0.378786796564403);
#1212=CIRCLE('',#16446,0.4);
#1213=CIRCLE('',#16449,0.378786796564403);
#1214=CIRCLE('',#16450,0.4);
#1215=CIRCLE('',#16454,0.4);
#1216=CIRCLE('',#16457,0.4);
#1217=CIRCLE('',#16461,0.361213203435596);
#1218=CIRCLE('',#16462,0.31);
#1219=CIRCLE('',#16465,0.361213203435596);
#1220=CIRCLE('',#16466,0.31);
#1221=CIRCLE('',#16475,0.363786796564403);
#1222=CIRCLE('',#16476,0.415);
#1223=CIRCLE('',#16481,0.363786796564403);
#1224=CIRCLE('',#16482,0.415);
#1225=CIRCLE('',#16486,0.361213203435596);
#1226=CIRCLE('',#16487,0.31);
#1227=CIRCLE('',#16490,0.361213203435596);
#1228=CIRCLE('',#16491,0.31);
#1229=CIRCLE('',#16495,0.363786796564403);
#1230=CIRCLE('',#16496,0.415);
#1231=CIRCLE('',#16501,0.363786796564403);
#1232=CIRCLE('',#16502,0.415);
#1233=CIRCLE('',#16505,1.75);
#1234=CIRCLE('',#16507,1.6);
#1235=CIRCLE('',#16508,1.6);
#1236=CIRCLE('',#16509,1.6);
#1237=CIRCLE('',#16511,1.5787867965644);
#1238=CIRCLE('',#16514,0.15);
#1239=CIRCLE('',#16519,0.4);
#1240=CIRCLE('',#16520,0.36);
#1241=CIRCLE('',#16523,0.4);
#1242=CIRCLE('',#16524,0.36);
#1243=CIRCLE('',#16528,0.365);
#1244=CIRCLE('',#16529,0.325);
#1245=CIRCLE('',#16533,0.365);
#1246=CIRCLE('',#16534,0.325);
#1247=CIRCLE('',#16538,0.365);
#1248=CIRCLE('',#16539,0.325);
#1249=CIRCLE('',#16543,0.365);
#1250=CIRCLE('',#16544,0.325);
#1251=CIRCLE('',#16547,0.36);
#1252=CIRCLE('',#16550,0.36);
#1253=CIRCLE('',#16552,0.325);
#1254=CIRCLE('',#16556,0.325);
#1255=CIRCLE('',#16560,0.4);
#1256=CIRCLE('',#16563,0.4);
#1257=CIRCLE('',#16568,0.325);
#1258=CIRCLE('',#16572,0.325);
#1259=CIRCLE('',#16583,0.435);
#1260=CIRCLE('',#16584,0.205);
#1261=CIRCLE('',#16586,0.205);
#1262=CIRCLE('',#16588,0.205);
#1263=CIRCLE('',#16589,0.205);
#1264=CIRCLE('',#16591,0.435);
#1265=CIRCLE('',#16592,0.205);
#1266=CIRCLE('',#16594,0.205);
#1267=CIRCLE('',#16600,0.205);
#1268=CIRCLE('',#16602,0.205);
#1269=CIRCLE('',#16605,0.95);
#1270=CIRCLE('',#16607,1.);
#1271=CIRCLE('',#16609,1.);
#1272=CIRCLE('',#16611,1.25);
#1273=CIRCLE('',#16613,1.3);
#1274=CIRCLE('',#16615,1.3);
#1275=CIRCLE('',#16617,1.24);
#1276=CIRCLE('',#16619,0.755);
#1277=CIRCLE('',#16621,0.705);
#1278=CIRCLE('',#16623,0.705);
#1279=CIRCLE('',#16627,0.619999999999999);
#1280=CIRCLE('',#16628,0.671213203435596);
#1281=CIRCLE('',#16629,0.671213203435596);
#1282=CIRCLE('',#16631,0.678786796564404);
#1283=CIRCLE('',#16632,0.678786796564404);
#1284=CIRCLE('',#16635,0.7);
#1285=CIRCLE('',#16636,0.7);
#1286=CIRCLE('',#16638,0.7);
#1287=CIRCLE('',#16639,0.7);
#1288=CIRCLE('',#16641,0.678786796564404);
#1289=CIRCLE('',#16642,0.678786796564404);
#1290=CIRCLE('',#16644,0.671213203435597);
#1291=CIRCLE('',#16645,0.671213203435597);
#1292=CIRCLE('',#16647,0.62);
#1293=CIRCLE('',#16685,0.254999999999999);
#1294=CIRCLE('',#16686,0.285);
#1295=CIRCLE('',#16687,0.285);
#1296=CIRCLE('',#16688,0.285);
#1297=CIRCLE('',#16689,0.255000000000001);
#1298=CIRCLE('',#16690,1.385);
#1299=CIRCLE('',#16697,1.1);
#1300=CIRCLE('',#16698,1.1);
#1301=CIRCLE('',#16699,1.1212132034356);
#1302=CIRCLE('',#16700,1.1212132034356);
#1303=CIRCLE('',#16702,1.1);
#1304=CIRCLE('',#16703,1.1);
#1305=CIRCLE('',#16705,1.1287867965644);
#1306=CIRCLE('',#16707,1.13);
#1307=CIRCLE('',#16709,1.26);
#1308=CIRCLE('',#16711,1.29);
#1309=CIRCLE('',#16712,1.26);
#1310=CIRCLE('',#16713,1.26);
#1311=CIRCLE('',#16715,1.355);
#1312=CIRCLE('',#16718,1.355);
#1313=CIRCLE('',#16721,0.225);
#1314=CIRCLE('',#16723,0.225);
#1315=CIRCLE('',#16724,0.225);
#1316=CIRCLE('',#16726,0.254999999999999);
#1317=CIRCLE('',#16728,0.4);
#1318=CIRCLE('',#16730,0.225000000000001);
#1319=CIRCLE('',#16732,0.225000000000001);
#1320=CIRCLE('',#16733,0.225000000000001);
#1321=CIRCLE('',#16735,0.255000000000001);
#1322=CIRCLE('',#16737,0.4);
#1323=CIRCLE('',#16739,0.255);
#1324=CIRCLE('',#16741,0.255);
#1325=CIRCLE('',#16743,0.255000000000001);
#1326=CIRCLE('',#16745,0.255000000000001);
#1327=CIRCLE('',#16747,0.255);
#1328=CIRCLE('',#16749,0.255);
#1329=CIRCLE('',#16751,0.430000000000001);
#1330=CIRCLE('',#16752,0.4);
#1331=CIRCLE('',#16754,0.43);
#1332=CIRCLE('',#16755,0.285);
#1333=CIRCLE('',#16756,0.285);
#1334=CIRCLE('',#16757,0.285);
#1335=CIRCLE('',#16758,1.18);
#1336=CIRCLE('',#16761,0.4);
#1337=CIRCLE('',#16776,1.22);
#1338=CIRCLE('',#16778,1.25);
#1339=CIRCLE('',#16780,1.25);
#1340=CIRCLE('',#16782,1.22);
#1341=CIRCLE('',#16788,1.286875);
#1342=CIRCLE('',#16790,1.286875);
#1343=CIRCLE('',#16792,1.3442);
#1344=CIRCLE('',#16794,1.3442);
#1345=CIRCLE('',#16795,1.286875);
#1346=CIRCLE('',#16797,1.3442);
#1347=CIRCLE('',#16799,1.286875);
#1348=CIRCLE('',#16802,1.3442);
#1349=CIRCLE('',#16803,1.3442);
#1350=CIRCLE('',#16807,1.3442);
#1351=CIRCLE('',#16809,1.3442);
#1352=CIRCLE('',#16811,1.05);
#1353=CIRCLE('',#16812,1.05);
#1354=CIRCLE('',#16815,1.05);
#1355=CIRCLE('',#16818,1.05);
#1356=CIRCLE('',#16819,1.05);
#1357=CIRCLE('',#16820,1.05);
#1358=CIRCLE('',#16822,1.31);
#1359=CIRCLE('',#16824,1.31);
#1360=CIRCLE('',#16826,1.08);
#1361=CIRCLE('',#16828,1.08);
#1362=CIRCLE('',#16832,1.32);
#1363=CIRCLE('',#16836,0.1954);
#1364=CIRCLE('',#16843,0.15555);
#1365=CIRCLE('',#16850,0.1954);
#1366=CIRCLE('',#16851,0.1954);
#1367=CIRCLE('',#16853,0.1954);
#1368=CIRCLE('',#16854,0.1954);
#1369=CIRCLE('',#16855,0.15555);
#1370=CIRCLE('',#16858,0.115470053837925);
#1371=CIRCLE('',#16860,0.115470053837925);
#1372=CIRCLE('',#16862,0.115470053837925);
#1373=CIRCLE('',#16864,0.115470053837925);
#1374=CIRCLE('',#16866,0.115470053837925);
#1375=CIRCLE('',#16868,0.115470053837925);
#1376=CIRCLE('',#16870,0.113827101150665);
#1377=CIRCLE('',#16871,0.113827101150665);
#1378=CIRCLE('',#16872,0.113827101150665);
#1379=CIRCLE('',#16873,0.113827101150665);
#1380=CIRCLE('',#16874,0.113827101150665);
#1381=CIRCLE('',#16875,0.113827101150665);
#1382=CIRCLE('',#16876,0.113827101150665);
#1383=CIRCLE('',#16902,0.125);
#1384=CIRCLE('',#16905,0.1954);
#1385=CIRCLE('',#16907,0.17);
#1386=CIRCLE('',#16911,0.1954);
#1387=CIRCLE('',#16917,0.15555);
#1388=CIRCLE('',#16919,0.15555);
#1389=CIRCLE('',#16924,0.1954);
#1390=CIRCLE('',#16925,0.1954);
#1391=CIRCLE('',#16927,0.1954);
#1392=CIRCLE('',#16928,0.1954);
#1393=CIRCLE('',#16929,0.15555);
#1394=CIRCLE('',#16932,0.115470053837925);
#1395=CIRCLE('',#16934,0.115470053837925);
#1396=CIRCLE('',#16936,0.115470053837925);
#1397=CIRCLE('',#16938,0.115470053837925);
#1398=CIRCLE('',#16940,0.115470053837925);
#1399=CIRCLE('',#16942,0.115470053837925);
#1400=CIRCLE('',#16944,0.113827101150665);
#1401=CIRCLE('',#16945,0.113827101150665);
#1402=CIRCLE('',#16946,0.113827101150665);
#1403=CIRCLE('',#16947,0.113827101150665);
#1404=CIRCLE('',#16948,0.113827101150665);
#1405=CIRCLE('',#16949,0.113827101150665);
#1406=CIRCLE('',#16950,0.113827101150665);
#1407=CIRCLE('',#16976,0.125);
#1408=CIRCLE('',#16979,0.1954);
#1409=CIRCLE('',#16981,0.17);
#1410=CIRCLE('',#16992,1.2);
#1411=CIRCLE('',#16993,1.2);
#1412=CIRCLE('',#16995,1.2);
#1413=CIRCLE('',#16997,1.2);
#1414=CIRCLE('',#17001,1.17);
#1415=CIRCLE('',#17003,1.1787867965644);
#1416=CIRCLE('',#17005,1.1712132034356);
#1417=CIRCLE('',#17007,0.7);
#1418=CIRCLE('',#17008,0.7);
#1419=CIRCLE('',#17010,1.12);
#1420=CIRCLE('',#17012,0.74);
#1421=CIRCLE('',#17031,0.13);
#1422=CIRCLE('',#17042,0.21);
#1423=CIRCLE('',#17043,0.234999999999999);
#1424=CIRCLE('',#17044,1.58);
#1425=CIRCLE('',#17045,0.235);
#1426=CIRCLE('',#17047,0.158786796564404);
#1427=CIRCLE('',#17050,0.205);
#1428=CIRCLE('',#17052,0.205);
#1429=CIRCLE('',#17054,0.205);
#1430=CIRCLE('',#17056,0.205);
#1431=CIRCLE('',#17058,0.1);
#1432=CIRCLE('',#17061,0.1);
#1433=CIRCLE('',#17062,0.13);
#1434=CIRCLE('',#17065,1.5287867965644);
#1435=CIRCLE('',#17067,1.5212132034356);
#1436=CIRCLE('',#17069,0.235);
#1437=CIRCLE('',#17071,0.234999999999999);
#1438=CIRCLE('',#17072,1.58);
#1439=CIRCLE('',#17080,1.5);
#1440=CIRCLE('',#17082,1.5);
#1441=CIRCLE('',#17084,1.5287867965644);
#1442=CIRCLE('',#17086,1.5212132034356);
#1443=CIRCLE('',#17100,0.24635);
#1444=CIRCLE('',#17124,0.24635);
#1445=CIRCLE('',#17126,0.217775);
#1446=CIRCLE('',#17155,0.151);
#1447=CIRCLE('',#17156,0.151);
#1448=CIRCLE('',#17159,0.24635);
#1449=CIRCLE('',#17160,0.24635);
#1450=CIRCLE('',#17161,0.217775);
#1451=CIRCLE('',#17224,0.5);
#1452=CIRCLE('',#17225,0.5);
#1453=CIRCLE('',#17227,0.5);
#1454=CIRCLE('',#17228,0.5);
#1455=CIRCLE('',#17230,0.5);
#1456=CIRCLE('',#17231,0.5);
#1457=CIRCLE('',#17233,0.5);
#1458=CIRCLE('',#17234,0.5);
#1459=CIRCLE('',#17236,0.5);
#1460=CIRCLE('',#17237,0.5);
#1461=CIRCLE('',#17239,0.5);
#1462=CIRCLE('',#17240,0.5);
#1463=CIRCLE('',#17242,0.5);
#1464=CIRCLE('',#17243,0.5);
#1465=CIRCLE('',#17245,0.5);
#1466=CIRCLE('',#17246,0.5);
#1467=CIRCLE('',#17248,0.5);
#1468=CIRCLE('',#17249,0.5);
#1469=CIRCLE('',#17251,0.5);
#1470=CIRCLE('',#17252,0.5);
#1471=CIRCLE('',#17254,0.5);
#1472=CIRCLE('',#17255,0.5);
#1473=CIRCLE('',#17257,0.5);
#1474=CIRCLE('',#17258,0.5);
#1475=CIRCLE('',#17260,0.5);
#1476=CIRCLE('',#17261,0.5);
#1477=CIRCLE('',#17263,0.5);
#1478=CIRCLE('',#17264,0.5);
#1479=CIRCLE('',#17266,0.5);
#1480=CIRCLE('',#17267,0.5);
#1481=CIRCLE('',#17269,0.5);
#1482=CIRCLE('',#17270,0.5);
#1483=CIRCLE('',#17272,0.5);
#1484=CIRCLE('',#17273,0.5);
#1485=CIRCLE('',#17275,0.5);
#1486=CIRCLE('',#17276,0.5);
#1487=CIRCLE('',#17278,0.5);
#1488=CIRCLE('',#17279,0.5);
#1489=CIRCLE('',#17281,0.5);
#1490=CIRCLE('',#17282,0.5);
#1491=CIRCLE('',#17284,0.5);
#1492=CIRCLE('',#17285,0.5);
#1493=CIRCLE('',#17287,0.5);
#1494=CIRCLE('',#17288,0.5);
#1495=CIRCLE('',#17290,0.5);
#1496=CIRCLE('',#17291,0.5);
#1497=CIRCLE('',#17293,0.5);
#1498=CIRCLE('',#17294,0.5);
#1499=CIRCLE('',#17296,0.5);
#1500=CIRCLE('',#17297,0.5);
#1501=CIRCLE('',#17299,0.5);
#1502=CIRCLE('',#17300,0.5);
#1503=CIRCLE('',#17302,0.5);
#1504=CIRCLE('',#17303,0.5);
#1505=CIRCLE('',#17305,0.5);
#1506=CIRCLE('',#17306,0.5);
#1507=CIRCLE('',#17308,0.5);
#1508=CIRCLE('',#17309,0.5);
#1509=CIRCLE('',#17311,0.5);
#1510=CIRCLE('',#17312,0.5);
#1511=CIRCLE('',#17314,0.45);
#1512=CIRCLE('',#17316,0.21);
#1513=CIRCLE('',#17319,0.24635);
#1514=CIRCLE('',#17322,0.44);
#1515=CIRCLE('',#17326,0.15);
#1516=CIRCLE('',#17328,0.03);
#1517=CIRCLE('',#17329,0.03);
#1518=CIRCLE('',#17334,0.1954);
#1519=CIRCLE('',#17357,0.15555);
#1520=CIRCLE('',#17380,0.1954);
#1521=CIRCLE('',#17381,0.1954);
#1522=CIRCLE('',#17383,0.1954);
#1523=CIRCLE('',#17384,0.1954);
#1524=CIRCLE('',#17385,0.15555);
#1525=CIRCLE('',#17388,0.02);
#1526=CIRCLE('',#17389,0.2154);
#1527=CIRCLE('',#17390,0.1954);
#1528=CIRCLE('',#17393,0.35);
#1529=CIRCLE('',#17394,0.35);
#1530=CIRCLE('',#17395,0.35);
#1531=CIRCLE('',#17396,0.35);
#1532=CIRCLE('',#17397,0.35);
#1533=CIRCLE('',#17398,0.35);
#1534=CIRCLE('',#17399,0.35);
#1535=CIRCLE('',#17400,0.35);
#1536=CIRCLE('',#17401,0.35);
#1537=CIRCLE('',#17402,0.35);
#1538=CIRCLE('',#17403,0.35);
#1539=CIRCLE('',#17404,0.35);
#1540=CIRCLE('',#17405,0.35);
#1541=CIRCLE('',#17406,0.35);
#1542=CIRCLE('',#17407,0.35);
#1543=CIRCLE('',#17408,0.35);
#1544=CIRCLE('',#17409,0.35);
#1545=CIRCLE('',#17410,0.35);
#1546=CIRCLE('',#17411,0.35);
#1547=CIRCLE('',#17412,0.35);
#1548=CIRCLE('',#17413,0.35);
#1549=CIRCLE('',#17414,0.35);
#1550=CIRCLE('',#17415,0.35);
#1551=CIRCLE('',#17416,0.35);
#1552=CIRCLE('',#17417,0.35);
#1553=CIRCLE('',#17418,0.35);
#1554=CIRCLE('',#17419,0.35);
#1555=CIRCLE('',#17420,0.35);
#1556=CIRCLE('',#17421,0.35);
#1557=CIRCLE('',#17422,0.35);
#1558=CIRCLE('',#17423,0.35);
#1559=CIRCLE('',#17424,0.35);
#1560=CIRCLE('',#17425,0.35);
#1561=CIRCLE('',#17426,0.35);
#1562=CIRCLE('',#17427,0.35);
#1563=CIRCLE('',#17428,0.35);
#1564=CIRCLE('',#17430,0.173205080756888);
#1565=CIRCLE('',#17432,0.173205080756888);
#1566=CIRCLE('',#17434,0.173205080756888);
#1567=CIRCLE('',#17436,0.173205080756888);
#1568=CIRCLE('',#17438,0.173205080756888);
#1569=CIRCLE('',#17440,0.173205080756888);
#1570=CIRCLE('',#17442,0.171554298747513);
#1571=CIRCLE('',#17443,0.171554298747513);
#1572=CIRCLE('',#17444,0.171554298747513);
#1573=CIRCLE('',#17445,0.171554298747513);
#1574=CIRCLE('',#17446,0.171554298747513);
#1575=CIRCLE('',#17447,0.171554298747513);
#1576=CIRCLE('',#17448,0.171554298747513);
#1577=CIRCLE('',#17546,0.35);
#1578=CIRCLE('',#17548,0.35);
#1579=CIRCLE('',#17550,0.35);
#1580=CIRCLE('',#17552,0.35);
#1581=CIRCLE('',#17554,0.35);
#1582=CIRCLE('',#17556,0.35);
#1583=CIRCLE('',#17558,0.35);
#1584=CIRCLE('',#17560,0.35);
#1585=CIRCLE('',#17562,0.35);
#1586=CIRCLE('',#17564,0.35);
#1587=CIRCLE('',#17566,0.35);
#1588=CIRCLE('',#17568,0.35);
#1589=CIRCLE('',#17570,0.35);
#1590=CIRCLE('',#17572,0.35);
#1591=CIRCLE('',#17574,0.35);
#1592=CIRCLE('',#17576,0.35);
#1593=CIRCLE('',#17578,0.35);
#1594=CIRCLE('',#17580,0.35);
#1595=CIRCLE('',#17582,0.35);
#1596=CIRCLE('',#17584,0.35);
#1597=CIRCLE('',#17586,0.35);
#1598=CIRCLE('',#17588,0.35);
#1599=CIRCLE('',#17590,0.35);
#1600=CIRCLE('',#17592,0.35);
#1601=CIRCLE('',#17594,0.35);
#1602=CIRCLE('',#17596,0.35);
#1603=CIRCLE('',#17598,0.35);
#1604=CIRCLE('',#17600,0.35);
#1605=CIRCLE('',#17602,0.35);
#1606=CIRCLE('',#17604,0.35);
#1607=CIRCLE('',#17606,0.35);
#1608=CIRCLE('',#17608,0.35);
#1609=CIRCLE('',#17610,0.35);
#1610=CIRCLE('',#17612,0.35);
#1611=CIRCLE('',#17614,0.35);
#1612=CIRCLE('',#17616,0.35);
#1613=CIRCLE('',#17618,0.16);
#1614=CIRCLE('',#17621,0.31);
#1615=CIRCLE('',#17625,0.1954);
#1616=CIRCLE('',#17637,0.15555);
#1617=CIRCLE('',#17649,0.1954);
#1618=CIRCLE('',#17650,0.1954);
#1619=CIRCLE('',#17651,0.15555);
#1620=CIRCLE('',#17702,0.4);
#1621=CIRCLE('',#17703,0.4);
#1622=CIRCLE('',#17705,0.4);
#1623=CIRCLE('',#17706,0.4);
#1624=CIRCLE('',#17708,0.4);
#1625=CIRCLE('',#17709,0.4);
#1626=CIRCLE('',#17711,0.4);
#1627=CIRCLE('',#17712,0.4);
#1628=CIRCLE('',#17714,0.4);
#1629=CIRCLE('',#17715,0.4);
#1630=CIRCLE('',#17717,0.4);
#1631=CIRCLE('',#17718,0.4);
#1632=CIRCLE('',#17720,0.4);
#1633=CIRCLE('',#17721,0.4);
#1634=CIRCLE('',#17723,0.4);
#1635=CIRCLE('',#17724,0.4);
#1636=CIRCLE('',#17726,0.4);
#1637=CIRCLE('',#17727,0.4);
#1638=CIRCLE('',#17729,0.4);
#1639=CIRCLE('',#17730,0.4);
#1640=CIRCLE('',#17732,0.4);
#1641=CIRCLE('',#17733,0.4);
#1642=CIRCLE('',#17735,0.4);
#1643=CIRCLE('',#17736,0.4);
#1644=CIRCLE('',#17738,0.4);
#1645=CIRCLE('',#17739,0.4);
#1646=CIRCLE('',#17741,0.4);
#1647=CIRCLE('',#17742,0.4);
#1648=CIRCLE('',#17744,0.4);
#1649=CIRCLE('',#17745,0.4);
#1650=CIRCLE('',#17747,0.4);
#1651=CIRCLE('',#17748,0.4);
#1652=CIRCLE('',#17750,0.4);
#1653=CIRCLE('',#17751,0.4);
#1654=CIRCLE('',#17753,0.4);
#1655=CIRCLE('',#17754,0.4);
#1656=CIRCLE('',#17756,0.4);
#1657=CIRCLE('',#17757,0.4);
#1658=CIRCLE('',#17759,0.4);
#1659=CIRCLE('',#17760,0.4);
#1660=CIRCLE('',#17762,0.4);
#1661=CIRCLE('',#17763,0.4);
#1662=CIRCLE('',#17765,0.4);
#1663=CIRCLE('',#17766,0.4);
#1664=CIRCLE('',#17768,0.4);
#1665=CIRCLE('',#17769,0.4);
#1666=CIRCLE('',#17771,0.4);
#1667=CIRCLE('',#17772,0.4);
#1668=CIRCLE('',#17774,0.36);
#1669=CIRCLE('',#17776,0.17);
#1670=CIRCLE('',#17779,0.1954);
#1671=CIRCLE('',#17782,0.35);
#1672=CONICAL_SURFACE('',#16424,1.0543933982822,1.17809724509618);
#1673=CONICAL_SURFACE('',#16427,1.025,0.785398163397448);
#1674=CONICAL_SURFACE('',#16431,1.0106066017178,0.392699081698721);
#1675=CONICAL_SURFACE('',#16444,0.389393398282202,0.392699081698728);
#1676=CONICAL_SURFACE('',#16448,0.389393398282202,0.392699081698728);
#1677=CONICAL_SURFACE('',#16460,0.335606601717798,1.17809724509618);
#1678=CONICAL_SURFACE('',#16464,0.335606601717798,1.17809724509618);
#1679=CONICAL_SURFACE('',#16469,0.37,0.785398163397451);
#1680=CONICAL_SURFACE('',#16471,0.37,0.785398163397451);
#1681=CONICAL_SURFACE('',#16474,0.389393398282202,1.17809724509617);
#1682=CONICAL_SURFACE('',#16480,0.389393398282202,1.17809724509617);
#1683=CONICAL_SURFACE('',#16485,0.335606601717798,1.17809724509618);
#1684=CONICAL_SURFACE('',#16489,0.335606601717798,1.17809724509618);
#1685=CONICAL_SURFACE('',#16494,0.389393398282202,1.17809724509617);
#1686=CONICAL_SURFACE('',#16500,0.389393398282202,1.17809724509617);
#1687=CONICAL_SURFACE('',#16510,1.5893933982822,0.392699081698725);
#1688=CONICAL_SURFACE('',#16512,1.57,0.785398163397448);
#1689=CONICAL_SURFACE('',#16518,0.38,0.785398163397451);
#1690=CONICAL_SURFACE('',#16522,0.38,0.785398163397451);
#1691=CONICAL_SURFACE('',#16527,0.345,0.785398163397448);
#1692=CONICAL_SURFACE('',#16532,0.345,0.785398163397448);
#1693=CONICAL_SURFACE('',#16537,0.345,0.785398163397448);
#1694=CONICAL_SURFACE('',#16542,0.345,0.785398163397448);
#1695=CONICAL_SURFACE('',#16546,0.38,0.785398163397451);
#1696=CONICAL_SURFACE('',#16549,0.38,0.785398163397451);
#1697=CONICAL_SURFACE('',#16559,0.37,0.785398163397451);
#1698=CONICAL_SURFACE('',#16562,0.37,0.785398163397451);
#1699=CONICAL_SURFACE('',#16565,0.355,0.785398163397448);
#1700=CONICAL_SURFACE('',#16567,0.355,0.785398163397448);
#1701=CONICAL_SURFACE('',#16569,0.355,0.785398163397448);
#1702=CONICAL_SURFACE('',#16571,0.355,0.785398163397448);
#1703=CONICAL_SURFACE('',#16585,0.2175,0.785398163397448);
#1704=CONICAL_SURFACE('',#16590,0.435,0.785398163397448);
#1705=CONICAL_SURFACE('',#16606,0.975,0.785398163397449);
#1706=CONICAL_SURFACE('',#16612,1.275,0.785398163397446);
#1707=CONICAL_SURFACE('',#16616,1.27,0.785398163397448);
#1708=CONICAL_SURFACE('',#16620,0.73,0.785398163397451);
#1709=CONICAL_SURFACE('',#16626,0.645606601717798,1.17809724509618);
#1710=CONICAL_SURFACE('',#16630,0.675,0.78539816339745);
#1711=CONICAL_SURFACE('',#16634,0.689393398282202,0.392699081698726);
#1712=CONICAL_SURFACE('',#16640,0.689393398282202,0.392699081698718);
#1713=CONICAL_SURFACE('',#16643,0.675,0.785398163397447);
#1714=CONICAL_SURFACE('',#16646,0.645606601717798,1.17809724509617);
#1715=CONICAL_SURFACE('',#16696,1.1106066017178,0.392699081698722);
#1716=CONICAL_SURFACE('',#16704,1.14,0.785398163397448);
#1717=CONICAL_SURFACE('',#16706,1.115,0.785398163397448);
#1718=CONICAL_SURFACE('',#16710,1.275,0.785398163397448);
#1719=CONICAL_SURFACE('',#16717,1.37,0.785398163397449);
#1720=CONICAL_SURFACE('',#16720,0.239999999999999,0.785398163397438);
#1721=CONICAL_SURFACE('',#16725,0.239999999999999,0.785398163397438);
#1722=CONICAL_SURFACE('',#16729,0.240000000000001,0.785398163397452);
#1723=CONICAL_SURFACE('',#16734,0.240000000000001,0.785398163397452);
#1724=CONICAL_SURFACE('',#16738,0.27,0.785398163397452);
#1725=CONICAL_SURFACE('',#16742,0.27,0.785398163397437);
#1726=CONICAL_SURFACE('',#16746,0.27,0.785398163397452);
#1727=CONICAL_SURFACE('',#16750,0.415,0.785398163397452);
#1728=CONICAL_SURFACE('',#16760,0.415,0.785398163397437);
#1729=CONICAL_SURFACE('',#16763,1.1543933982822,1.17809724509617);
#1730=CONICAL_SURFACE('',#16768,0.27,0.785398163397452);
#1731=CONICAL_SURFACE('',#16769,0.27,0.785398163397437);
#1732=CONICAL_SURFACE('',#16770,0.27,0.785398163397452);
#1733=CONICAL_SURFACE('',#16777,1.235,0.785398163397449);
#1734=CONICAL_SURFACE('',#16781,1.235,0.78539816339745);
#1735=CONICAL_SURFACE('',#16821,1.33,0.785398163397449);
#1736=CONICAL_SURFACE('',#16823,1.33,0.785398163397449);
#1737=CONICAL_SURFACE('',#16829,1.065,0.785398163397447);
#1738=CONICAL_SURFACE('',#16830,1.065,0.785398163397447);
#1739=CONICAL_SURFACE('',#16831,1.335,0.785398163397448);
#1740=CONICAL_SURFACE('',#16869,0.0577350269189626,1.02403331474479);
#1741=CONICAL_SURFACE('',#16903,0.1625,0.982793723247329);
#1742=CONICAL_SURFACE('',#16906,0.185,0.785398163397449);
#1743=CONICAL_SURFACE('',#16943,0.0577350269189626,1.02403331474479);
#1744=CONICAL_SURFACE('',#16977,0.1625,0.982793723247329);
#1745=CONICAL_SURFACE('',#16980,0.185,0.785398163397449);
#1746=CONICAL_SURFACE('',#17000,1.185,0.785398163397445);
#1747=CONICAL_SURFACE('',#17002,1.1893933982822,0.392699081698718);
#1748=CONICAL_SURFACE('',#17004,1.175,0.785398163397451);
#1749=CONICAL_SURFACE('',#17009,1.1456066017178,1.17809724509618);
#1750=CONICAL_SURFACE('',#17046,0.184393398282202,1.17809724509617);
#1751=CONICAL_SURFACE('',#17048,0.115,0.785398163397448);
#1752=CONICAL_SURFACE('',#17049,0.22,0.785398163397453);
#1753=CONICAL_SURFACE('',#17053,0.22,0.785398163397438);
#1754=CONICAL_SURFACE('',#17057,0.115,0.785398163397456);
#1755=CONICAL_SURFACE('',#17060,0.115,0.785398163397456);
#1756=CONICAL_SURFACE('',#17064,1.5543933982822,1.17809724509617);
#1757=CONICAL_SURFACE('',#17066,1.525,0.785398163397449);
#1758=CONICAL_SURFACE('',#17068,0.22,0.785398163397452);
#1759=CONICAL_SURFACE('',#17073,0.22,0.785398163397437);
#1760=CONICAL_SURFACE('',#17079,1.5106066017178,0.392699081698724);
#1761=CONICAL_SURFACE('',#17083,1.5543933982822,1.17809724509617);
#1762=CONICAL_SURFACE('',#17085,1.525,0.785398163397448);
#1763=CONICAL_SURFACE('',#17087,1.5106066017178,0.392699081698721);
#1764=CONICAL_SURFACE('',#17090,0.72,0.785398163397448);
#1765=CONICAL_SURFACE('',#17313,0.475,0.785398163397448);
#1766=CONICAL_SURFACE('',#17317,0.23,0.785398163397448);
#1767=CONICAL_SURFACE('',#17321,0.47,0.785398163397448);
#1768=CONICAL_SURFACE('',#17441,0.0866025403784439,1.02614241494116);
#1769=CONICAL_SURFACE('',#17619,0.18,0.785398163397448);
#1770=CONICAL_SURFACE('',#17620,0.33,0.785398163397448);
#1771=CONICAL_SURFACE('',#17773,0.38,0.785398163397449);
#1772=CONICAL_SURFACE('',#17777,0.185,0.785398163397448);
#1773=CONICAL_SURFACE('',#17781,0.375,0.785398163397449);
#1774=FACE_OUTER_BOUND('',#2691,.T.);
#1775=FACE_OUTER_BOUND('',#2692,.T.);
#1776=FACE_OUTER_BOUND('',#2693,.T.);
#1777=FACE_OUTER_BOUND('',#2694,.T.);
#1778=FACE_OUTER_BOUND('',#2695,.T.);
#1779=FACE_OUTER_BOUND('',#2696,.T.);
#1780=FACE_OUTER_BOUND('',#2697,.T.);
#1781=FACE_OUTER_BOUND('',#2698,.T.);
#1782=FACE_OUTER_BOUND('',#2699,.T.);
#1783=FACE_OUTER_BOUND('',#2700,.T.);
#1784=FACE_OUTER_BOUND('',#2701,.T.);
#1785=FACE_OUTER_BOUND('',#2702,.T.);
#1786=FACE_OUTER_BOUND('',#2703,.T.);
#1787=FACE_OUTER_BOUND('',#2704,.T.);
#1788=FACE_OUTER_BOUND('',#2705,.T.);
#1789=FACE_OUTER_BOUND('',#2706,.T.);
#1790=FACE_OUTER_BOUND('',#2707,.T.);
#1791=FACE_OUTER_BOUND('',#2708,.T.);
#1792=FACE_OUTER_BOUND('',#2709,.T.);
#1793=FACE_OUTER_BOUND('',#2710,.T.);
#1794=FACE_OUTER_BOUND('',#2711,.T.);
#1795=FACE_OUTER_BOUND('',#2712,.T.);
#1796=FACE_OUTER_BOUND('',#2714,.T.);
#1797=FACE_OUTER_BOUND('',#2715,.T.);
#1798=FACE_OUTER_BOUND('',#2717,.T.);
#1799=FACE_OUTER_BOUND('',#2718,.T.);
#1800=FACE_OUTER_BOUND('',#2719,.T.);
#1801=FACE_OUTER_BOUND('',#2720,.T.);
#1802=FACE_OUTER_BOUND('',#2721,.T.);
#1803=FACE_OUTER_BOUND('',#2722,.T.);
#1804=FACE_OUTER_BOUND('',#2723,.T.);
#1805=FACE_OUTER_BOUND('',#2724,.T.);
#1806=FACE_OUTER_BOUND('',#2725,.T.);
#1807=FACE_OUTER_BOUND('',#2726,.T.);
#1808=FACE_OUTER_BOUND('',#2727,.T.);
#1809=FACE_OUTER_BOUND('',#2728,.T.);
#1810=FACE_OUTER_BOUND('',#2729,.T.);
#1811=FACE_OUTER_BOUND('',#2730,.T.);
#1812=FACE_OUTER_BOUND('',#2731,.T.);
#1813=FACE_OUTER_BOUND('',#2732,.T.);
#1814=FACE_OUTER_BOUND('',#2733,.T.);
#1815=FACE_OUTER_BOUND('',#2734,.T.);
#1816=FACE_OUTER_BOUND('',#2735,.T.);
#1817=FACE_OUTER_BOUND('',#2736,.T.);
#1818=FACE_OUTER_BOUND('',#2737,.T.);
#1819=FACE_OUTER_BOUND('',#2738,.T.);
#1820=FACE_OUTER_BOUND('',#2739,.T.);
#1821=FACE_OUTER_BOUND('',#2740,.T.);
#1822=FACE_OUTER_BOUND('',#2741,.T.);
#1823=FACE_OUTER_BOUND('',#2742,.T.);
#1824=FACE_OUTER_BOUND('',#2743,.T.);
#1825=FACE_OUTER_BOUND('',#2744,.T.);
#1826=FACE_OUTER_BOUND('',#2745,.T.);
#1827=FACE_OUTER_BOUND('',#2746,.T.);
#1828=FACE_OUTER_BOUND('',#2747,.T.);
#1829=FACE_OUTER_BOUND('',#2748,.T.);
#1830=FACE_OUTER_BOUND('',#2749,.T.);
#1831=FACE_OUTER_BOUND('',#2750,.T.);
#1832=FACE_OUTER_BOUND('',#2751,.T.);
#1833=FACE_OUTER_BOUND('',#2752,.T.);
#1834=FACE_OUTER_BOUND('',#2753,.T.);
#1835=FACE_OUTER_BOUND('',#2754,.T.);
#1836=FACE_OUTER_BOUND('',#2755,.T.);
#1837=FACE_OUTER_BOUND('',#2756,.T.);
#1838=FACE_OUTER_BOUND('',#2757,.T.);
#1839=FACE_OUTER_BOUND('',#2758,.T.);
#1840=FACE_OUTER_BOUND('',#2759,.T.);
#1841=FACE_OUTER_BOUND('',#2760,.T.);
#1842=FACE_OUTER_BOUND('',#2761,.T.);
#1843=FACE_OUTER_BOUND('',#2762,.T.);
#1844=FACE_OUTER_BOUND('',#2763,.T.);
#1845=FACE_OUTER_BOUND('',#2764,.T.);
#1846=FACE_OUTER_BOUND('',#2765,.T.);
#1847=FACE_OUTER_BOUND('',#2767,.T.);
#1848=FACE_OUTER_BOUND('',#2768,.T.);
#1849=FACE_OUTER_BOUND('',#2770,.T.);
#1850=FACE_OUTER_BOUND('',#2771,.T.);
#1851=FACE_OUTER_BOUND('',#2772,.T.);
#1852=FACE_OUTER_BOUND('',#2773,.T.);
#1853=FACE_OUTER_BOUND('',#2774,.T.);
#1854=FACE_OUTER_BOUND('',#2775,.T.);
#1855=FACE_OUTER_BOUND('',#2776,.T.);
#1856=FACE_OUTER_BOUND('',#2777,.T.);
#1857=FACE_OUTER_BOUND('',#2778,.T.);
#1858=FACE_OUTER_BOUND('',#2779,.T.);
#1859=FACE_OUTER_BOUND('',#2780,.T.);
#1860=FACE_OUTER_BOUND('',#2781,.T.);
#1861=FACE_OUTER_BOUND('',#2782,.T.);
#1862=FACE_OUTER_BOUND('',#2783,.T.);
#1863=FACE_OUTER_BOUND('',#2784,.T.);
#1864=FACE_OUTER_BOUND('',#2785,.T.);
#1865=FACE_OUTER_BOUND('',#2786,.T.);
#1866=FACE_OUTER_BOUND('',#2787,.T.);
#1867=FACE_OUTER_BOUND('',#2788,.T.);
#1868=FACE_OUTER_BOUND('',#2789,.T.);
#1869=FACE_OUTER_BOUND('',#2790,.T.);
#1870=FACE_OUTER_BOUND('',#2791,.T.);
#1871=FACE_OUTER_BOUND('',#2792,.T.);
#1872=FACE_OUTER_BOUND('',#2793,.T.);
#1873=FACE_OUTER_BOUND('',#2794,.T.);
#1874=FACE_OUTER_BOUND('',#2795,.T.);
#1875=FACE_OUTER_BOUND('',#2796,.T.);
#1876=FACE_OUTER_BOUND('',#2797,.T.);
#1877=FACE_OUTER_BOUND('',#2798,.T.);
#1878=FACE_OUTER_BOUND('',#2799,.T.);
#1879=FACE_OUTER_BOUND('',#2800,.T.);
#1880=FACE_OUTER_BOUND('',#2801,.T.);
#1881=FACE_OUTER_BOUND('',#2802,.T.);
#1882=FACE_OUTER_BOUND('',#2803,.T.);
#1883=FACE_OUTER_BOUND('',#2804,.T.);
#1884=FACE_OUTER_BOUND('',#2805,.T.);
#1885=FACE_OUTER_BOUND('',#2806,.T.);
#1886=FACE_OUTER_BOUND('',#2807,.T.);
#1887=FACE_OUTER_BOUND('',#2808,.T.);
#1888=FACE_OUTER_BOUND('',#2809,.T.);
#1889=FACE_OUTER_BOUND('',#2810,.T.);
#1890=FACE_OUTER_BOUND('',#2811,.T.);
#1891=FACE_OUTER_BOUND('',#2812,.T.);
#1892=FACE_OUTER_BOUND('',#2813,.T.);
#1893=FACE_OUTER_BOUND('',#2814,.T.);
#1894=FACE_OUTER_BOUND('',#2815,.T.);
#1895=FACE_OUTER_BOUND('',#2816,.T.);
#1896=FACE_OUTER_BOUND('',#2817,.T.);
#1897=FACE_OUTER_BOUND('',#2818,.T.);
#1898=FACE_OUTER_BOUND('',#2819,.T.);
#1899=FACE_OUTER_BOUND('',#2821,.T.);
#1900=FACE_OUTER_BOUND('',#2822,.T.);
#1901=FACE_OUTER_BOUND('',#2823,.T.);
#1902=FACE_OUTER_BOUND('',#2824,.T.);
#1903=FACE_OUTER_BOUND('',#2826,.T.);
#1904=FACE_OUTER_BOUND('',#2827,.T.);
#1905=FACE_OUTER_BOUND('',#2828,.T.);
#1906=FACE_OUTER_BOUND('',#2829,.T.);
#1907=FACE_OUTER_BOUND('',#2830,.T.);
#1908=FACE_OUTER_BOUND('',#2831,.T.);
#1909=FACE_OUTER_BOUND('',#2832,.T.);
#1910=FACE_OUTER_BOUND('',#2833,.T.);
#1911=FACE_OUTER_BOUND('',#2834,.T.);
#1912=FACE_OUTER_BOUND('',#2835,.T.);
#1913=FACE_OUTER_BOUND('',#2836,.T.);
#1914=FACE_OUTER_BOUND('',#2838,.T.);
#1915=FACE_OUTER_BOUND('',#2839,.T.);
#1916=FACE_OUTER_BOUND('',#2841,.T.);
#1917=FACE_OUTER_BOUND('',#2842,.T.);
#1918=FACE_OUTER_BOUND('',#2844,.T.);
#1919=FACE_OUTER_BOUND('',#2845,.T.);
#1920=FACE_OUTER_BOUND('',#2847,.T.);
#1921=FACE_OUTER_BOUND('',#2848,.T.);
#1922=FACE_OUTER_BOUND('',#2849,.T.);
#1923=FACE_OUTER_BOUND('',#2850,.T.);
#1924=FACE_OUTER_BOUND('',#2851,.T.);
#1925=FACE_OUTER_BOUND('',#2852,.T.);
#1926=FACE_OUTER_BOUND('',#2853,.T.);
#1927=FACE_OUTER_BOUND('',#2854,.T.);
#1928=FACE_OUTER_BOUND('',#2855,.T.);
#1929=FACE_OUTER_BOUND('',#2856,.T.);
#1930=FACE_OUTER_BOUND('',#2857,.T.);
#1931=FACE_OUTER_BOUND('',#2858,.T.);
#1932=FACE_OUTER_BOUND('',#2859,.T.);
#1933=FACE_OUTER_BOUND('',#2860,.T.);
#1934=FACE_OUTER_BOUND('',#2861,.T.);
#1935=FACE_OUTER_BOUND('',#2862,.T.);
#1936=FACE_OUTER_BOUND('',#2863,.T.);
#1937=FACE_OUTER_BOUND('',#2864,.T.);
#1938=FACE_OUTER_BOUND('',#2865,.T.);
#1939=FACE_OUTER_BOUND('',#2866,.T.);
#1940=FACE_OUTER_BOUND('',#2867,.T.);
#1941=FACE_OUTER_BOUND('',#2868,.T.);
#1942=FACE_OUTER_BOUND('',#2869,.T.);
#1943=FACE_OUTER_BOUND('',#2870,.T.);
#1944=FACE_OUTER_BOUND('',#2871,.T.);
#1945=FACE_OUTER_BOUND('',#2872,.T.);
#1946=FACE_OUTER_BOUND('',#2873,.T.);
#1947=FACE_OUTER_BOUND('',#2874,.T.);
#1948=FACE_OUTER_BOUND('',#2875,.T.);
#1949=FACE_OUTER_BOUND('',#2876,.T.);
#1950=FACE_OUTER_BOUND('',#2877,.T.);
#1951=FACE_OUTER_BOUND('',#2878,.T.);
#1952=FACE_OUTER_BOUND('',#2879,.T.);
#1953=FACE_OUTER_BOUND('',#2880,.T.);
#1954=FACE_OUTER_BOUND('',#2881,.T.);
#1955=FACE_OUTER_BOUND('',#2882,.T.);
#1956=FACE_OUTER_BOUND('',#2883,.T.);
#1957=FACE_OUTER_BOUND('',#2884,.T.);
#1958=FACE_OUTER_BOUND('',#2885,.T.);
#1959=FACE_OUTER_BOUND('',#2886,.T.);
#1960=FACE_OUTER_BOUND('',#2887,.T.);
#1961=FACE_OUTER_BOUND('',#2888,.T.);
#1962=FACE_OUTER_BOUND('',#2889,.T.);
#1963=FACE_OUTER_BOUND('',#2890,.T.);
#1964=FACE_OUTER_BOUND('',#2891,.T.);
#1965=FACE_OUTER_BOUND('',#2898,.T.);
#1966=FACE_OUTER_BOUND('',#2899,.T.);
#1967=FACE_OUTER_BOUND('',#2900,.T.);
#1968=FACE_OUTER_BOUND('',#2901,.T.);
#1969=FACE_OUTER_BOUND('',#2902,.T.);
#1970=FACE_OUTER_BOUND('',#2903,.T.);
#1971=FACE_OUTER_BOUND('',#2904,.T.);
#1972=FACE_OUTER_BOUND('',#2905,.T.);
#1973=FACE_OUTER_BOUND('',#2906,.T.);
#1974=FACE_OUTER_BOUND('',#2907,.T.);
#1975=FACE_OUTER_BOUND('',#2909,.T.);
#1976=FACE_OUTER_BOUND('',#2910,.T.);
#1977=FACE_OUTER_BOUND('',#2912,.T.);
#1978=FACE_OUTER_BOUND('',#2913,.T.);
#1979=FACE_OUTER_BOUND('',#2914,.T.);
#1980=FACE_OUTER_BOUND('',#2915,.T.);
#1981=FACE_OUTER_BOUND('',#2916,.T.);
#1982=FACE_OUTER_BOUND('',#2917,.T.);
#1983=FACE_OUTER_BOUND('',#2918,.T.);
#1984=FACE_OUTER_BOUND('',#2920,.T.);
#1985=FACE_OUTER_BOUND('',#2921,.T.);
#1986=FACE_OUTER_BOUND('',#2922,.T.);
#1987=FACE_OUTER_BOUND('',#2923,.T.);
#1988=FACE_OUTER_BOUND('',#2925,.T.);
#1989=FACE_OUTER_BOUND('',#2926,.T.);
#1990=FACE_OUTER_BOUND('',#2927,.T.);
#1991=FACE_OUTER_BOUND('',#2928,.T.);
#1992=FACE_OUTER_BOUND('',#2929,.T.);
#1993=FACE_OUTER_BOUND('',#2930,.T.);
#1994=FACE_OUTER_BOUND('',#2931,.T.);
#1995=FACE_OUTER_BOUND('',#2932,.T.);
#1996=FACE_OUTER_BOUND('',#2939,.T.);
#1997=FACE_OUTER_BOUND('',#2940,.T.);
#1998=FACE_OUTER_BOUND('',#2941,.T.);
#1999=FACE_OUTER_BOUND('',#2942,.T.);
#2000=FACE_OUTER_BOUND('',#2943,.T.);
#2001=FACE_OUTER_BOUND('',#2944,.T.);
#2002=FACE_OUTER_BOUND('',#2945,.T.);
#2003=FACE_OUTER_BOUND('',#2946,.T.);
#2004=FACE_OUTER_BOUND('',#2947,.T.);
#2005=FACE_OUTER_BOUND('',#2948,.T.);
#2006=FACE_OUTER_BOUND('',#2949,.T.);
#2007=FACE_OUTER_BOUND('',#2950,.T.);
#2008=FACE_OUTER_BOUND('',#2951,.T.);
#2009=FACE_OUTER_BOUND('',#2952,.T.);
#2010=FACE_OUTER_BOUND('',#2953,.T.);
#2011=FACE_OUTER_BOUND('',#2954,.T.);
#2012=FACE_OUTER_BOUND('',#2955,.T.);
#2013=FACE_OUTER_BOUND('',#2956,.T.);
#2014=FACE_OUTER_BOUND('',#2957,.T.);
#2015=FACE_OUTER_BOUND('',#2958,.T.);
#2016=FACE_OUTER_BOUND('',#2959,.T.);
#2017=FACE_OUTER_BOUND('',#2960,.T.);
#2018=FACE_OUTER_BOUND('',#2961,.T.);
#2019=FACE_OUTER_BOUND('',#2962,.T.);
#2020=FACE_OUTER_BOUND('',#2963,.T.);
#2021=FACE_OUTER_BOUND('',#2964,.T.);
#2022=FACE_OUTER_BOUND('',#2965,.T.);
#2023=FACE_OUTER_BOUND('',#2966,.T.);
#2024=FACE_OUTER_BOUND('',#2967,.T.);
#2025=FACE_OUTER_BOUND('',#2968,.T.);
#2026=FACE_OUTER_BOUND('',#2969,.T.);
#2027=FACE_OUTER_BOUND('',#2970,.T.);
#2028=FACE_OUTER_BOUND('',#2971,.T.);
#2029=FACE_OUTER_BOUND('',#2972,.T.);
#2030=FACE_OUTER_BOUND('',#2973,.T.);
#2031=FACE_OUTER_BOUND('',#2974,.T.);
#2032=FACE_OUTER_BOUND('',#2975,.T.);
#2033=FACE_OUTER_BOUND('',#2976,.T.);
#2034=FACE_OUTER_BOUND('',#2977,.T.);
#2035=FACE_OUTER_BOUND('',#2978,.T.);
#2036=FACE_OUTER_BOUND('',#2979,.T.);
#2037=FACE_OUTER_BOUND('',#2980,.T.);
#2038=FACE_OUTER_BOUND('',#2981,.T.);
#2039=FACE_OUTER_BOUND('',#2982,.T.);
#2040=FACE_OUTER_BOUND('',#2983,.T.);
#2041=FACE_OUTER_BOUND('',#2984,.T.);
#2042=FACE_OUTER_BOUND('',#2985,.T.);
#2043=FACE_OUTER_BOUND('',#2986,.T.);
#2044=FACE_OUTER_BOUND('',#2987,.T.);
#2045=FACE_OUTER_BOUND('',#2988,.T.);
#2046=FACE_OUTER_BOUND('',#2989,.T.);
#2047=FACE_OUTER_BOUND('',#2991,.T.);
#2048=FACE_OUTER_BOUND('',#2992,.T.);
#2049=FACE_OUTER_BOUND('',#2993,.T.);
#2050=FACE_OUTER_BOUND('',#2994,.T.);
#2051=FACE_OUTER_BOUND('',#2995,.T.);
#2052=FACE_OUTER_BOUND('',#2996,.T.);
#2053=FACE_OUTER_BOUND('',#2997,.T.);
#2054=FACE_OUTER_BOUND('',#2998,.T.);
#2055=FACE_OUTER_BOUND('',#2999,.T.);
#2056=FACE_OUTER_BOUND('',#3000,.T.);
#2057=FACE_OUTER_BOUND('',#3001,.T.);
#2058=FACE_OUTER_BOUND('',#3002,.T.);
#2059=FACE_OUTER_BOUND('',#3003,.T.);
#2060=FACE_OUTER_BOUND('',#3004,.T.);
#2061=FACE_OUTER_BOUND('',#3005,.T.);
#2062=FACE_OUTER_BOUND('',#3006,.T.);
#2063=FACE_OUTER_BOUND('',#3007,.T.);
#2064=FACE_OUTER_BOUND('',#3008,.T.);
#2065=FACE_OUTER_BOUND('',#3009,.T.);
#2066=FACE_OUTER_BOUND('',#3010,.T.);
#2067=FACE_OUTER_BOUND('',#3011,.T.);
#2068=FACE_OUTER_BOUND('',#3012,.T.);
#2069=FACE_OUTER_BOUND('',#3013,.T.);
#2070=FACE_OUTER_BOUND('',#3014,.T.);
#2071=FACE_OUTER_BOUND('',#3015,.T.);
#2072=FACE_OUTER_BOUND('',#3016,.T.);
#2073=FACE_OUTER_BOUND('',#3017,.T.);
#2074=FACE_OUTER_BOUND('',#3018,.T.);
#2075=FACE_OUTER_BOUND('',#3019,.T.);
#2076=FACE_OUTER_BOUND('',#3020,.T.);
#2077=FACE_OUTER_BOUND('',#3021,.T.);
#2078=FACE_OUTER_BOUND('',#3022,.T.);
#2079=FACE_OUTER_BOUND('',#3023,.T.);
#2080=FACE_OUTER_BOUND('',#3024,.T.);
#2081=FACE_OUTER_BOUND('',#3025,.T.);
#2082=FACE_OUTER_BOUND('',#3026,.T.);
#2083=FACE_OUTER_BOUND('',#3027,.T.);
#2084=FACE_OUTER_BOUND('',#3028,.T.);
#2085=FACE_OUTER_BOUND('',#3029,.T.);
#2086=FACE_OUTER_BOUND('',#3030,.T.);
#2087=FACE_OUTER_BOUND('',#3031,.T.);
#2088=FACE_OUTER_BOUND('',#3032,.T.);
#2089=FACE_OUTER_BOUND('',#3033,.T.);
#2090=FACE_OUTER_BOUND('',#3034,.T.);
#2091=FACE_OUTER_BOUND('',#3035,.T.);
#2092=FACE_OUTER_BOUND('',#3036,.T.);
#2093=FACE_OUTER_BOUND('',#3037,.T.);
#2094=FACE_OUTER_BOUND('',#3038,.T.);
#2095=FACE_OUTER_BOUND('',#3039,.T.);
#2096=FACE_OUTER_BOUND('',#3040,.T.);
#2097=FACE_OUTER_BOUND('',#3041,.T.);
#2098=FACE_OUTER_BOUND('',#3042,.T.);
#2099=FACE_OUTER_BOUND('',#3043,.T.);
#2100=FACE_OUTER_BOUND('',#3045,.T.);
#2101=FACE_OUTER_BOUND('',#3046,.T.);
#2102=FACE_OUTER_BOUND('',#3047,.T.);
#2103=FACE_OUTER_BOUND('',#3048,.T.);
#2104=FACE_OUTER_BOUND('',#3049,.T.);
#2105=FACE_OUTER_BOUND('',#3050,.T.);
#2106=FACE_OUTER_BOUND('',#3051,.T.);
#2107=FACE_OUTER_BOUND('',#3052,.T.);
#2108=FACE_OUTER_BOUND('',#3053,.T.);
#2109=FACE_OUTER_BOUND('',#3054,.T.);
#2110=FACE_OUTER_BOUND('',#3055,.T.);
#2111=FACE_OUTER_BOUND('',#3056,.T.);
#2112=FACE_OUTER_BOUND('',#3057,.T.);
#2113=FACE_OUTER_BOUND('',#3058,.T.);
#2114=FACE_OUTER_BOUND('',#3059,.T.);
#2115=FACE_OUTER_BOUND('',#3060,.T.);
#2116=FACE_OUTER_BOUND('',#3061,.T.);
#2117=FACE_OUTER_BOUND('',#3062,.T.);
#2118=FACE_OUTER_BOUND('',#3063,.T.);
#2119=FACE_OUTER_BOUND('',#3064,.T.);
#2120=FACE_OUTER_BOUND('',#3065,.T.);
#2121=FACE_OUTER_BOUND('',#3066,.T.);
#2122=FACE_OUTER_BOUND('',#3067,.T.);
#2123=FACE_OUTER_BOUND('',#3068,.T.);
#2124=FACE_OUTER_BOUND('',#3069,.T.);
#2125=FACE_OUTER_BOUND('',#3070,.T.);
#2126=FACE_OUTER_BOUND('',#3071,.T.);
#2127=FACE_OUTER_BOUND('',#3072,.T.);
#2128=FACE_OUTER_BOUND('',#3073,.T.);
#2129=FACE_OUTER_BOUND('',#3074,.T.);
#2130=FACE_OUTER_BOUND('',#3075,.T.);
#2131=FACE_OUTER_BOUND('',#3076,.T.);
#2132=FACE_OUTER_BOUND('',#3077,.T.);
#2133=FACE_OUTER_BOUND('',#3078,.T.);
#2134=FACE_OUTER_BOUND('',#3079,.T.);
#2135=FACE_OUTER_BOUND('',#3080,.T.);
#2136=FACE_OUTER_BOUND('',#3081,.T.);
#2137=FACE_OUTER_BOUND('',#3082,.T.);
#2138=FACE_OUTER_BOUND('',#3083,.T.);
#2139=FACE_OUTER_BOUND('',#3084,.T.);
#2140=FACE_OUTER_BOUND('',#3085,.T.);
#2141=FACE_OUTER_BOUND('',#3086,.T.);
#2142=FACE_OUTER_BOUND('',#3087,.T.);
#2143=FACE_OUTER_BOUND('',#3088,.T.);
#2144=FACE_OUTER_BOUND('',#3089,.T.);
#2145=FACE_OUTER_BOUND('',#3090,.T.);
#2146=FACE_OUTER_BOUND('',#3091,.T.);
#2147=FACE_OUTER_BOUND('',#3092,.T.);
#2148=FACE_OUTER_BOUND('',#3093,.T.);
#2149=FACE_OUTER_BOUND('',#3094,.T.);
#2150=FACE_OUTER_BOUND('',#3095,.T.);
#2151=FACE_OUTER_BOUND('',#3097,.T.);
#2152=FACE_OUTER_BOUND('',#3098,.T.);
#2153=FACE_OUTER_BOUND('',#3099,.T.);
#2154=FACE_OUTER_BOUND('',#3100,.T.);
#2155=FACE_OUTER_BOUND('',#3101,.T.);
#2156=FACE_OUTER_BOUND('',#3102,.T.);
#2157=FACE_OUTER_BOUND('',#3103,.T.);
#2158=FACE_OUTER_BOUND('',#3104,.T.);
#2159=FACE_OUTER_BOUND('',#3105,.T.);
#2160=FACE_OUTER_BOUND('',#3106,.T.);
#2161=FACE_OUTER_BOUND('',#3108,.T.);
#2162=FACE_OUTER_BOUND('',#3109,.T.);
#2163=FACE_OUTER_BOUND('',#3110,.T.);
#2164=FACE_OUTER_BOUND('',#3111,.T.);
#2165=FACE_OUTER_BOUND('',#3112,.T.);
#2166=FACE_OUTER_BOUND('',#3113,.T.);
#2167=FACE_OUTER_BOUND('',#3115,.T.);
#2168=FACE_OUTER_BOUND('',#3116,.T.);
#2169=FACE_OUTER_BOUND('',#3118,.T.);
#2170=FACE_OUTER_BOUND('',#3119,.T.);
#2171=FACE_OUTER_BOUND('',#3120,.T.);
#2172=FACE_OUTER_BOUND('',#3121,.T.);
#2173=FACE_OUTER_BOUND('',#3122,.T.);
#2174=FACE_OUTER_BOUND('',#3123,.T.);
#2175=FACE_OUTER_BOUND('',#3124,.T.);
#2176=FACE_OUTER_BOUND('',#3125,.T.);
#2177=FACE_OUTER_BOUND('',#3126,.T.);
#2178=FACE_OUTER_BOUND('',#3127,.T.);
#2179=FACE_OUTER_BOUND('',#3128,.T.);
#2180=FACE_OUTER_BOUND('',#3129,.T.);
#2181=FACE_OUTER_BOUND('',#3130,.T.);
#2182=FACE_OUTER_BOUND('',#3131,.T.);
#2183=FACE_OUTER_BOUND('',#3132,.T.);
#2184=FACE_OUTER_BOUND('',#3133,.T.);
#2185=FACE_OUTER_BOUND('',#3134,.T.);
#2186=FACE_OUTER_BOUND('',#3135,.T.);
#2187=FACE_OUTER_BOUND('',#3136,.T.);
#2188=FACE_OUTER_BOUND('',#3137,.T.);
#2189=FACE_OUTER_BOUND('',#3138,.T.);
#2190=FACE_OUTER_BOUND('',#3139,.T.);
#2191=FACE_OUTER_BOUND('',#3140,.T.);
#2192=FACE_OUTER_BOUND('',#3141,.T.);
#2193=FACE_OUTER_BOUND('',#3142,.T.);
#2194=FACE_OUTER_BOUND('',#3143,.T.);
#2195=FACE_OUTER_BOUND('',#3144,.T.);
#2196=FACE_OUTER_BOUND('',#3145,.T.);
#2197=FACE_OUTER_BOUND('',#3151,.T.);
#2198=FACE_OUTER_BOUND('',#3152,.T.);
#2199=FACE_OUTER_BOUND('',#3153,.T.);
#2200=FACE_OUTER_BOUND('',#3154,.T.);
#2201=FACE_OUTER_BOUND('',#3155,.T.);
#2202=FACE_OUTER_BOUND('',#3156,.T.);
#2203=FACE_OUTER_BOUND('',#3157,.T.);
#2204=FACE_OUTER_BOUND('',#3158,.T.);
#2205=FACE_OUTER_BOUND('',#3159,.T.);
#2206=FACE_OUTER_BOUND('',#3160,.T.);
#2207=FACE_OUTER_BOUND('',#3161,.T.);
#2208=FACE_OUTER_BOUND('',#3162,.T.);
#2209=FACE_OUTER_BOUND('',#3163,.T.);
#2210=FACE_OUTER_BOUND('',#3164,.T.);
#2211=FACE_OUTER_BOUND('',#3168,.T.);
#2212=FACE_OUTER_BOUND('',#3169,.T.);
#2213=FACE_OUTER_BOUND('',#3170,.T.);
#2214=FACE_OUTER_BOUND('',#3171,.T.);
#2215=FACE_OUTER_BOUND('',#3172,.T.);
#2216=FACE_OUTER_BOUND('',#3173,.T.);
#2217=FACE_OUTER_BOUND('',#3174,.T.);
#2218=FACE_OUTER_BOUND('',#3175,.T.);
#2219=FACE_OUTER_BOUND('',#3176,.T.);
#2220=FACE_OUTER_BOUND('',#3177,.T.);
#2221=FACE_OUTER_BOUND('',#3178,.T.);
#2222=FACE_OUTER_BOUND('',#3179,.T.);
#2223=FACE_OUTER_BOUND('',#3180,.T.);
#2224=FACE_OUTER_BOUND('',#3181,.T.);
#2225=FACE_OUTER_BOUND('',#3182,.T.);
#2226=FACE_OUTER_BOUND('',#3183,.T.);
#2227=FACE_OUTER_BOUND('',#3184,.T.);
#2228=FACE_OUTER_BOUND('',#3185,.T.);
#2229=FACE_OUTER_BOUND('',#3186,.T.);
#2230=FACE_OUTER_BOUND('',#3187,.T.);
#2231=FACE_OUTER_BOUND('',#3188,.T.);
#2232=FACE_OUTER_BOUND('',#3189,.T.);
#2233=FACE_OUTER_BOUND('',#3190,.T.);
#2234=FACE_OUTER_BOUND('',#3191,.T.);
#2235=FACE_OUTER_BOUND('',#3192,.T.);
#2236=FACE_OUTER_BOUND('',#3193,.T.);
#2237=FACE_OUTER_BOUND('',#3194,.T.);
#2238=FACE_OUTER_BOUND('',#3195,.T.);
#2239=FACE_OUTER_BOUND('',#3196,.T.);
#2240=FACE_OUTER_BOUND('',#3197,.T.);
#2241=FACE_OUTER_BOUND('',#3198,.T.);
#2242=FACE_OUTER_BOUND('',#3199,.T.);
#2243=FACE_OUTER_BOUND('',#3200,.T.);
#2244=FACE_OUTER_BOUND('',#3201,.T.);
#2245=FACE_OUTER_BOUND('',#3202,.T.);
#2246=FACE_OUTER_BOUND('',#3203,.T.);
#2247=FACE_OUTER_BOUND('',#3204,.T.);
#2248=FACE_OUTER_BOUND('',#3205,.T.);
#2249=FACE_OUTER_BOUND('',#3206,.T.);
#2250=FACE_OUTER_BOUND('',#3207,.T.);
#2251=FACE_OUTER_BOUND('',#3208,.T.);
#2252=FACE_OUTER_BOUND('',#3209,.T.);
#2253=FACE_OUTER_BOUND('',#3210,.T.);
#2254=FACE_OUTER_BOUND('',#3211,.T.);
#2255=FACE_OUTER_BOUND('',#3212,.T.);
#2256=FACE_OUTER_BOUND('',#3213,.T.);
#2257=FACE_OUTER_BOUND('',#3214,.T.);
#2258=FACE_OUTER_BOUND('',#3215,.T.);
#2259=FACE_OUTER_BOUND('',#3216,.T.);
#2260=FACE_OUTER_BOUND('',#3217,.T.);
#2261=FACE_OUTER_BOUND('',#3218,.T.);
#2262=FACE_OUTER_BOUND('',#3219,.T.);
#2263=FACE_OUTER_BOUND('',#3220,.T.);
#2264=FACE_OUTER_BOUND('',#3221,.T.);
#2265=FACE_OUTER_BOUND('',#3222,.T.);
#2266=FACE_OUTER_BOUND('',#3223,.T.);
#2267=FACE_OUTER_BOUND('',#3224,.T.);
#2268=FACE_OUTER_BOUND('',#3225,.T.);
#2269=FACE_OUTER_BOUND('',#3226,.T.);
#2270=FACE_OUTER_BOUND('',#3227,.T.);
#2271=FACE_OUTER_BOUND('',#3228,.T.);
#2272=FACE_OUTER_BOUND('',#3229,.T.);
#2273=FACE_OUTER_BOUND('',#3230,.T.);
#2274=FACE_OUTER_BOUND('',#3231,.T.);
#2275=FACE_OUTER_BOUND('',#3232,.T.);
#2276=FACE_OUTER_BOUND('',#3233,.T.);
#2277=FACE_OUTER_BOUND('',#3234,.T.);
#2278=FACE_OUTER_BOUND('',#3235,.T.);
#2279=FACE_OUTER_BOUND('',#3236,.T.);
#2280=FACE_OUTER_BOUND('',#3237,.T.);
#2281=FACE_OUTER_BOUND('',#3238,.T.);
#2282=FACE_OUTER_BOUND('',#3239,.T.);
#2283=FACE_OUTER_BOUND('',#3240,.T.);
#2284=FACE_OUTER_BOUND('',#3241,.T.);
#2285=FACE_OUTER_BOUND('',#3242,.T.);
#2286=FACE_OUTER_BOUND('',#3243,.T.);
#2287=FACE_OUTER_BOUND('',#3244,.T.);
#2288=FACE_OUTER_BOUND('',#3245,.T.);
#2289=FACE_OUTER_BOUND('',#3246,.T.);
#2290=FACE_OUTER_BOUND('',#3247,.T.);
#2291=FACE_OUTER_BOUND('',#3248,.T.);
#2292=FACE_OUTER_BOUND('',#3249,.T.);
#2293=FACE_OUTER_BOUND('',#3250,.T.);
#2294=FACE_OUTER_BOUND('',#3251,.T.);
#2295=FACE_OUTER_BOUND('',#3252,.T.);
#2296=FACE_OUTER_BOUND('',#3253,.T.);
#2297=FACE_OUTER_BOUND('',#3254,.T.);
#2298=FACE_OUTER_BOUND('',#3255,.T.);
#2299=FACE_OUTER_BOUND('',#3256,.T.);
#2300=FACE_OUTER_BOUND('',#3257,.T.);
#2301=FACE_OUTER_BOUND('',#3258,.T.);
#2302=FACE_OUTER_BOUND('',#3259,.T.);
#2303=FACE_OUTER_BOUND('',#3260,.T.);
#2304=FACE_OUTER_BOUND('',#3261,.T.);
#2305=FACE_OUTER_BOUND('',#3262,.T.);
#2306=FACE_OUTER_BOUND('',#3263,.T.);
#2307=FACE_OUTER_BOUND('',#3264,.T.);
#2308=FACE_OUTER_BOUND('',#3265,.T.);
#2309=FACE_OUTER_BOUND('',#3266,.T.);
#2310=FACE_OUTER_BOUND('',#3267,.T.);
#2311=FACE_OUTER_BOUND('',#3268,.T.);
#2312=FACE_OUTER_BOUND('',#3269,.T.);
#2313=FACE_OUTER_BOUND('',#3270,.T.);
#2314=FACE_OUTER_BOUND('',#3271,.T.);
#2315=FACE_OUTER_BOUND('',#3272,.T.);
#2316=FACE_OUTER_BOUND('',#3273,.T.);
#2317=FACE_OUTER_BOUND('',#3274,.T.);
#2318=FACE_OUTER_BOUND('',#3275,.T.);
#2319=FACE_OUTER_BOUND('',#3276,.T.);
#2320=FACE_OUTER_BOUND('',#3277,.T.);
#2321=FACE_OUTER_BOUND('',#3278,.T.);
#2322=FACE_OUTER_BOUND('',#3279,.T.);
#2323=FACE_OUTER_BOUND('',#3280,.T.);
#2324=FACE_OUTER_BOUND('',#3281,.T.);
#2325=FACE_OUTER_BOUND('',#3282,.T.);
#2326=FACE_OUTER_BOUND('',#3283,.T.);
#2327=FACE_OUTER_BOUND('',#3284,.T.);
#2328=FACE_OUTER_BOUND('',#3285,.T.);
#2329=FACE_OUTER_BOUND('',#3286,.T.);
#2330=FACE_OUTER_BOUND('',#3287,.T.);
#2331=FACE_OUTER_BOUND('',#3288,.T.);
#2332=FACE_OUTER_BOUND('',#3289,.T.);
#2333=FACE_OUTER_BOUND('',#3290,.T.);
#2334=FACE_OUTER_BOUND('',#3291,.T.);
#2335=FACE_OUTER_BOUND('',#3292,.T.);
#2336=FACE_OUTER_BOUND('',#3293,.T.);
#2337=FACE_OUTER_BOUND('',#3294,.T.);
#2338=FACE_OUTER_BOUND('',#3295,.T.);
#2339=FACE_OUTER_BOUND('',#3296,.T.);
#2340=FACE_OUTER_BOUND('',#3297,.T.);
#2341=FACE_OUTER_BOUND('',#3298,.T.);
#2342=FACE_OUTER_BOUND('',#3299,.T.);
#2343=FACE_OUTER_BOUND('',#3300,.T.);
#2344=FACE_OUTER_BOUND('',#3301,.T.);
#2345=FACE_OUTER_BOUND('',#3302,.T.);
#2346=FACE_OUTER_BOUND('',#3303,.T.);
#2347=FACE_OUTER_BOUND('',#3304,.T.);
#2348=FACE_OUTER_BOUND('',#3305,.T.);
#2349=FACE_OUTER_BOUND('',#3306,.T.);
#2350=FACE_OUTER_BOUND('',#3307,.T.);
#2351=FACE_OUTER_BOUND('',#3308,.T.);
#2352=FACE_OUTER_BOUND('',#3309,.T.);
#2353=FACE_OUTER_BOUND('',#3310,.T.);
#2354=FACE_OUTER_BOUND('',#3311,.T.);
#2355=FACE_OUTER_BOUND('',#3312,.T.);
#2356=FACE_OUTER_BOUND('',#3313,.T.);
#2357=FACE_OUTER_BOUND('',#3314,.T.);
#2358=FACE_OUTER_BOUND('',#3315,.T.);
#2359=FACE_OUTER_BOUND('',#3316,.T.);
#2360=FACE_OUTER_BOUND('',#3317,.T.);
#2361=FACE_OUTER_BOUND('',#3318,.T.);
#2362=FACE_OUTER_BOUND('',#3319,.T.);
#2363=FACE_OUTER_BOUND('',#3320,.T.);
#2364=FACE_OUTER_BOUND('',#3321,.T.);
#2365=FACE_OUTER_BOUND('',#3322,.T.);
#2366=FACE_OUTER_BOUND('',#3323,.T.);
#2367=FACE_OUTER_BOUND('',#3324,.T.);
#2368=FACE_OUTER_BOUND('',#3325,.T.);
#2369=FACE_OUTER_BOUND('',#3326,.T.);
#2370=FACE_OUTER_BOUND('',#3327,.T.);
#2371=FACE_OUTER_BOUND('',#3328,.T.);
#2372=FACE_OUTER_BOUND('',#3329,.T.);
#2373=FACE_OUTER_BOUND('',#3330,.T.);
#2374=FACE_OUTER_BOUND('',#3331,.T.);
#2375=FACE_OUTER_BOUND('',#3332,.T.);
#2376=FACE_OUTER_BOUND('',#3333,.T.);
#2377=FACE_OUTER_BOUND('',#3334,.T.);
#2378=FACE_OUTER_BOUND('',#3335,.T.);
#2379=FACE_OUTER_BOUND('',#3336,.T.);
#2380=FACE_OUTER_BOUND('',#3337,.T.);
#2381=FACE_OUTER_BOUND('',#3338,.T.);
#2382=FACE_OUTER_BOUND('',#3340,.T.);
#2383=FACE_OUTER_BOUND('',#3341,.T.);
#2384=FACE_OUTER_BOUND('',#3342,.T.);
#2385=FACE_OUTER_BOUND('',#3344,.T.);
#2386=FACE_OUTER_BOUND('',#3345,.T.);
#2387=FACE_OUTER_BOUND('',#3347,.T.);
#2388=FACE_OUTER_BOUND('',#3348,.T.);
#2389=FACE_OUTER_BOUND('',#3349,.T.);
#2390=FACE_OUTER_BOUND('',#3350,.T.);
#2391=FACE_OUTER_BOUND('',#3351,.T.);
#2392=FACE_OUTER_BOUND('',#3352,.T.);
#2393=FACE_OUTER_BOUND('',#3353,.T.);
#2394=FACE_OUTER_BOUND('',#3354,.T.);
#2395=FACE_OUTER_BOUND('',#3355,.T.);
#2396=FACE_OUTER_BOUND('',#3356,.T.);
#2397=FACE_OUTER_BOUND('',#3357,.T.);
#2398=FACE_OUTER_BOUND('',#3358,.T.);
#2399=FACE_OUTER_BOUND('',#3359,.T.);
#2400=FACE_OUTER_BOUND('',#3360,.T.);
#2401=FACE_OUTER_BOUND('',#3361,.T.);
#2402=FACE_OUTER_BOUND('',#3362,.T.);
#2403=FACE_OUTER_BOUND('',#3363,.T.);
#2404=FACE_OUTER_BOUND('',#3364,.T.);
#2405=FACE_OUTER_BOUND('',#3365,.T.);
#2406=FACE_OUTER_BOUND('',#3366,.T.);
#2407=FACE_OUTER_BOUND('',#3367,.T.);
#2408=FACE_OUTER_BOUND('',#3368,.T.);
#2409=FACE_OUTER_BOUND('',#3369,.T.);
#2410=FACE_OUTER_BOUND('',#3370,.T.);
#2411=FACE_OUTER_BOUND('',#3371,.T.);
#2412=FACE_OUTER_BOUND('',#3372,.T.);
#2413=FACE_OUTER_BOUND('',#3373,.T.);
#2414=FACE_OUTER_BOUND('',#3374,.T.);
#2415=FACE_OUTER_BOUND('',#3375,.T.);
#2416=FACE_OUTER_BOUND('',#3376,.T.);
#2417=FACE_OUTER_BOUND('',#3377,.T.);
#2418=FACE_OUTER_BOUND('',#3378,.T.);
#2419=FACE_OUTER_BOUND('',#3379,.T.);
#2420=FACE_OUTER_BOUND('',#3380,.T.);
#2421=FACE_OUTER_BOUND('',#3381,.T.);
#2422=FACE_OUTER_BOUND('',#3382,.T.);
#2423=FACE_OUTER_BOUND('',#3383,.T.);
#2424=FACE_OUTER_BOUND('',#3384,.T.);
#2425=FACE_OUTER_BOUND('',#3385,.T.);
#2426=FACE_OUTER_BOUND('',#3386,.T.);
#2427=FACE_OUTER_BOUND('',#3387,.T.);
#2428=FACE_OUTER_BOUND('',#3388,.T.);
#2429=FACE_OUTER_BOUND('',#3389,.T.);
#2430=FACE_OUTER_BOUND('',#3390,.T.);
#2431=FACE_OUTER_BOUND('',#3391,.T.);
#2432=FACE_OUTER_BOUND('',#3392,.T.);
#2433=FACE_OUTER_BOUND('',#3393,.T.);
#2434=FACE_OUTER_BOUND('',#3394,.T.);
#2435=FACE_OUTER_BOUND('',#3395,.T.);
#2436=FACE_OUTER_BOUND('',#3396,.T.);
#2437=FACE_OUTER_BOUND('',#3397,.T.);
#2438=FACE_OUTER_BOUND('',#3398,.T.);
#2439=FACE_OUTER_BOUND('',#3399,.T.);
#2440=FACE_OUTER_BOUND('',#3400,.T.);
#2441=FACE_OUTER_BOUND('',#3401,.T.);
#2442=FACE_OUTER_BOUND('',#3402,.T.);
#2443=FACE_OUTER_BOUND('',#3404,.T.);
#2444=FACE_OUTER_BOUND('',#3405,.T.);
#2445=FACE_OUTER_BOUND('',#3406,.T.);
#2446=FACE_OUTER_BOUND('',#3407,.T.);
#2447=FACE_OUTER_BOUND('',#3408,.T.);
#2448=FACE_OUTER_BOUND('',#3409,.T.);
#2449=FACE_OUTER_BOUND('',#3410,.T.);
#2450=FACE_OUTER_BOUND('',#3411,.T.);
#2451=FACE_OUTER_BOUND('',#3412,.T.);
#2452=FACE_OUTER_BOUND('',#3413,.T.);
#2453=FACE_OUTER_BOUND('',#3414,.T.);
#2454=FACE_OUTER_BOUND('',#3415,.T.);
#2455=FACE_OUTER_BOUND('',#3416,.T.);
#2456=FACE_OUTER_BOUND('',#3417,.T.);
#2457=FACE_OUTER_BOUND('',#3418,.T.);
#2458=FACE_OUTER_BOUND('',#3419,.T.);
#2459=FACE_OUTER_BOUND('',#3420,.T.);
#2460=FACE_OUTER_BOUND('',#3421,.T.);
#2461=FACE_OUTER_BOUND('',#3422,.T.);
#2462=FACE_OUTER_BOUND('',#3423,.T.);
#2463=FACE_OUTER_BOUND('',#3424,.T.);
#2464=FACE_OUTER_BOUND('',#3425,.T.);
#2465=FACE_OUTER_BOUND('',#3426,.T.);
#2466=FACE_OUTER_BOUND('',#3427,.T.);
#2467=FACE_OUTER_BOUND('',#3428,.T.);
#2468=FACE_OUTER_BOUND('',#3429,.T.);
#2469=FACE_OUTER_BOUND('',#3430,.T.);
#2470=FACE_OUTER_BOUND('',#3431,.T.);
#2471=FACE_OUTER_BOUND('',#3432,.T.);
#2472=FACE_OUTER_BOUND('',#3433,.T.);
#2473=FACE_OUTER_BOUND('',#3434,.T.);
#2474=FACE_OUTER_BOUND('',#3435,.T.);
#2475=FACE_OUTER_BOUND('',#3436,.T.);
#2476=FACE_OUTER_BOUND('',#3437,.T.);
#2477=FACE_OUTER_BOUND('',#3438,.T.);
#2478=FACE_OUTER_BOUND('',#3439,.T.);
#2479=FACE_OUTER_BOUND('',#3440,.T.);
#2480=FACE_OUTER_BOUND('',#3441,.T.);
#2481=FACE_OUTER_BOUND('',#3442,.T.);
#2482=FACE_OUTER_BOUND('',#3443,.T.);
#2483=FACE_OUTER_BOUND('',#3444,.T.);
#2484=FACE_OUTER_BOUND('',#3445,.T.);
#2485=FACE_OUTER_BOUND('',#3446,.T.);
#2486=FACE_OUTER_BOUND('',#3447,.T.);
#2487=FACE_OUTER_BOUND('',#3448,.T.);
#2488=FACE_OUTER_BOUND('',#3449,.T.);
#2489=FACE_OUTER_BOUND('',#3450,.T.);
#2490=FACE_OUTER_BOUND('',#3451,.T.);
#2491=FACE_OUTER_BOUND('',#3452,.T.);
#2492=FACE_OUTER_BOUND('',#3453,.T.);
#2493=FACE_OUTER_BOUND('',#3454,.T.);
#2494=FACE_OUTER_BOUND('',#3455,.T.);
#2495=FACE_OUTER_BOUND('',#3456,.T.);
#2496=FACE_OUTER_BOUND('',#3457,.T.);
#2497=FACE_OUTER_BOUND('',#3458,.T.);
#2498=FACE_OUTER_BOUND('',#3459,.T.);
#2499=FACE_OUTER_BOUND('',#3460,.T.);
#2500=FACE_OUTER_BOUND('',#3461,.T.);
#2501=FACE_OUTER_BOUND('',#3462,.T.);
#2502=FACE_OUTER_BOUND('',#3463,.T.);
#2503=FACE_OUTER_BOUND('',#3464,.T.);
#2504=FACE_OUTER_BOUND('',#3465,.T.);
#2505=FACE_OUTER_BOUND('',#3466,.T.);
#2506=FACE_OUTER_BOUND('',#3467,.T.);
#2507=FACE_OUTER_BOUND('',#3468,.T.);
#2508=FACE_OUTER_BOUND('',#3469,.T.);
#2509=FACE_OUTER_BOUND('',#3470,.T.);
#2510=FACE_OUTER_BOUND('',#3471,.T.);
#2511=FACE_OUTER_BOUND('',#3472,.T.);
#2512=FACE_OUTER_BOUND('',#3473,.T.);
#2513=FACE_OUTER_BOUND('',#3474,.T.);
#2514=FACE_OUTER_BOUND('',#3475,.T.);
#2515=FACE_OUTER_BOUND('',#3476,.T.);
#2516=FACE_OUTER_BOUND('',#3477,.T.);
#2517=FACE_OUTER_BOUND('',#3478,.T.);
#2518=FACE_OUTER_BOUND('',#3479,.T.);
#2519=FACE_OUTER_BOUND('',#3480,.T.);
#2520=FACE_OUTER_BOUND('',#3481,.T.);
#2521=FACE_OUTER_BOUND('',#3482,.T.);
#2522=FACE_OUTER_BOUND('',#3483,.T.);
#2523=FACE_OUTER_BOUND('',#3484,.T.);
#2524=FACE_OUTER_BOUND('',#3485,.T.);
#2525=FACE_OUTER_BOUND('',#3486,.T.);
#2526=FACE_OUTER_BOUND('',#3487,.T.);
#2527=FACE_OUTER_BOUND('',#3488,.T.);
#2528=FACE_OUTER_BOUND('',#3489,.T.);
#2529=FACE_OUTER_BOUND('',#3490,.T.);
#2530=FACE_OUTER_BOUND('',#3491,.T.);
#2531=FACE_OUTER_BOUND('',#3492,.T.);
#2532=FACE_OUTER_BOUND('',#3493,.T.);
#2533=FACE_OUTER_BOUND('',#3494,.T.);
#2534=FACE_OUTER_BOUND('',#3495,.T.);
#2535=FACE_OUTER_BOUND('',#3496,.T.);
#2536=FACE_OUTER_BOUND('',#3497,.T.);
#2537=FACE_OUTER_BOUND('',#3498,.T.);
#2538=FACE_OUTER_BOUND('',#3499,.T.);
#2539=FACE_OUTER_BOUND('',#3500,.T.);
#2540=FACE_OUTER_BOUND('',#3501,.T.);
#2541=FACE_OUTER_BOUND('',#3502,.T.);
#2542=FACE_OUTER_BOUND('',#3503,.T.);
#2543=FACE_OUTER_BOUND('',#3504,.T.);
#2544=FACE_OUTER_BOUND('',#3505,.T.);
#2545=FACE_OUTER_BOUND('',#3506,.T.);
#2546=FACE_OUTER_BOUND('',#3507,.T.);
#2547=FACE_OUTER_BOUND('',#3508,.T.);
#2548=FACE_OUTER_BOUND('',#3509,.T.);
#2549=FACE_OUTER_BOUND('',#3510,.T.);
#2550=FACE_OUTER_BOUND('',#3511,.T.);
#2551=FACE_OUTER_BOUND('',#3512,.T.);
#2552=FACE_OUTER_BOUND('',#3513,.T.);
#2553=FACE_OUTER_BOUND('',#3514,.T.);
#2554=FACE_OUTER_BOUND('',#3515,.T.);
#2555=FACE_OUTER_BOUND('',#3516,.T.);
#2556=FACE_OUTER_BOUND('',#3517,.T.);
#2557=FACE_OUTER_BOUND('',#3518,.T.);
#2558=FACE_OUTER_BOUND('',#3519,.T.);
#2559=FACE_OUTER_BOUND('',#3520,.T.);
#2560=FACE_OUTER_BOUND('',#3521,.T.);
#2561=FACE_OUTER_BOUND('',#3522,.T.);
#2562=FACE_OUTER_BOUND('',#3523,.T.);
#2563=FACE_OUTER_BOUND('',#3524,.T.);
#2564=FACE_OUTER_BOUND('',#3525,.T.);
#2565=FACE_OUTER_BOUND('',#3526,.T.);
#2566=FACE_OUTER_BOUND('',#3527,.T.);
#2567=FACE_OUTER_BOUND('',#3528,.T.);
#2568=FACE_OUTER_BOUND('',#3529,.T.);
#2569=FACE_OUTER_BOUND('',#3530,.T.);
#2570=FACE_OUTER_BOUND('',#3531,.T.);
#2571=FACE_OUTER_BOUND('',#3532,.T.);
#2572=FACE_OUTER_BOUND('',#3533,.T.);
#2573=FACE_OUTER_BOUND('',#3534,.T.);
#2574=FACE_OUTER_BOUND('',#3535,.T.);
#2575=FACE_OUTER_BOUND('',#3536,.T.);
#2576=FACE_OUTER_BOUND('',#3537,.T.);
#2577=FACE_OUTER_BOUND('',#3538,.T.);
#2578=FACE_OUTER_BOUND('',#3539,.T.);
#2579=FACE_OUTER_BOUND('',#3540,.T.);
#2580=FACE_OUTER_BOUND('',#3541,.T.);
#2581=FACE_OUTER_BOUND('',#3542,.T.);
#2582=FACE_OUTER_BOUND('',#3543,.T.);
#2583=FACE_OUTER_BOUND('',#3544,.T.);
#2584=FACE_OUTER_BOUND('',#3545,.T.);
#2585=FACE_OUTER_BOUND('',#3546,.T.);
#2586=FACE_OUTER_BOUND('',#3548,.T.);
#2587=FACE_OUTER_BOUND('',#3549,.T.);
#2588=FACE_OUTER_BOUND('',#3550,.T.);
#2589=FACE_OUTER_BOUND('',#3551,.T.);
#2590=FACE_OUTER_BOUND('',#3552,.T.);
#2591=FACE_OUTER_BOUND('',#3553,.T.);
#2592=FACE_OUTER_BOUND('',#3554,.T.);
#2593=FACE_OUTER_BOUND('',#3555,.T.);
#2594=FACE_OUTER_BOUND('',#3556,.T.);
#2595=FACE_OUTER_BOUND('',#3557,.T.);
#2596=FACE_OUTER_BOUND('',#3558,.T.);
#2597=FACE_OUTER_BOUND('',#3559,.T.);
#2598=FACE_OUTER_BOUND('',#3560,.T.);
#2599=FACE_OUTER_BOUND('',#3561,.T.);
#2600=FACE_OUTER_BOUND('',#3562,.T.);
#2601=FACE_OUTER_BOUND('',#3563,.T.);
#2602=FACE_OUTER_BOUND('',#3564,.T.);
#2603=FACE_OUTER_BOUND('',#3565,.T.);
#2604=FACE_OUTER_BOUND('',#3566,.T.);
#2605=FACE_OUTER_BOUND('',#3567,.T.);
#2606=FACE_OUTER_BOUND('',#3568,.T.);
#2607=FACE_OUTER_BOUND('',#3569,.T.);
#2608=FACE_OUTER_BOUND('',#3570,.T.);
#2609=FACE_OUTER_BOUND('',#3571,.T.);
#2610=FACE_OUTER_BOUND('',#3572,.T.);
#2611=FACE_OUTER_BOUND('',#3573,.T.);
#2612=FACE_OUTER_BOUND('',#3574,.T.);
#2613=FACE_OUTER_BOUND('',#3575,.T.);
#2614=FACE_OUTER_BOUND('',#3576,.T.);
#2615=FACE_OUTER_BOUND('',#3577,.T.);
#2616=FACE_OUTER_BOUND('',#3578,.T.);
#2617=FACE_OUTER_BOUND('',#3579,.T.);
#2618=FACE_OUTER_BOUND('',#3580,.T.);
#2619=FACE_OUTER_BOUND('',#3581,.T.);
#2620=FACE_OUTER_BOUND('',#3582,.T.);
#2621=FACE_OUTER_BOUND('',#3583,.T.);
#2622=FACE_OUTER_BOUND('',#3584,.T.);
#2623=FACE_OUTER_BOUND('',#3585,.T.);
#2624=FACE_OUTER_BOUND('',#3586,.T.);
#2625=FACE_OUTER_BOUND('',#3587,.T.);
#2626=FACE_OUTER_BOUND('',#3588,.T.);
#2627=FACE_OUTER_BOUND('',#3589,.T.);
#2628=FACE_OUTER_BOUND('',#3590,.T.);
#2629=FACE_OUTER_BOUND('',#3591,.T.);
#2630=FACE_OUTER_BOUND('',#3592,.T.);
#2631=FACE_OUTER_BOUND('',#3593,.T.);
#2632=FACE_OUTER_BOUND('',#3594,.T.);
#2633=FACE_OUTER_BOUND('',#3595,.T.);
#2634=FACE_OUTER_BOUND('',#3596,.T.);
#2635=FACE_OUTER_BOUND('',#3597,.T.);
#2636=FACE_OUTER_BOUND('',#3598,.T.);
#2637=FACE_OUTER_BOUND('',#3599,.T.);
#2638=FACE_OUTER_BOUND('',#3600,.T.);
#2639=FACE_OUTER_BOUND('',#3601,.T.);
#2640=FACE_OUTER_BOUND('',#3602,.T.);
#2641=FACE_OUTER_BOUND('',#3603,.T.);
#2642=FACE_OUTER_BOUND('',#3604,.T.);
#2643=FACE_OUTER_BOUND('',#3605,.T.);
#2644=FACE_OUTER_BOUND('',#3606,.T.);
#2645=FACE_OUTER_BOUND('',#3607,.T.);
#2646=FACE_OUTER_BOUND('',#3608,.T.);
#2647=FACE_OUTER_BOUND('',#3609,.T.);
#2648=FACE_OUTER_BOUND('',#3610,.T.);
#2649=FACE_OUTER_BOUND('',#3611,.T.);
#2650=FACE_OUTER_BOUND('',#3612,.T.);
#2651=FACE_OUTER_BOUND('',#3613,.T.);
#2652=FACE_OUTER_BOUND('',#3614,.T.);
#2653=FACE_OUTER_BOUND('',#3615,.T.);
#2654=FACE_OUTER_BOUND('',#3616,.T.);
#2655=FACE_OUTER_BOUND('',#3617,.T.);
#2656=FACE_OUTER_BOUND('',#3618,.T.);
#2657=FACE_OUTER_BOUND('',#3619,.T.);
#2658=FACE_OUTER_BOUND('',#3620,.T.);
#2659=FACE_OUTER_BOUND('',#3621,.T.);
#2660=FACE_OUTER_BOUND('',#3622,.T.);
#2661=FACE_OUTER_BOUND('',#3623,.T.);
#2662=FACE_OUTER_BOUND('',#3624,.T.);
#2663=FACE_OUTER_BOUND('',#3625,.T.);
#2664=FACE_OUTER_BOUND('',#3626,.T.);
#2665=FACE_OUTER_BOUND('',#3627,.T.);
#2666=FACE_OUTER_BOUND('',#3628,.T.);
#2667=FACE_OUTER_BOUND('',#3629,.T.);
#2668=FACE_OUTER_BOUND('',#3630,.T.);
#2669=FACE_OUTER_BOUND('',#3631,.T.);
#2670=FACE_OUTER_BOUND('',#3632,.T.);
#2671=FACE_OUTER_BOUND('',#3633,.T.);
#2672=FACE_OUTER_BOUND('',#3634,.T.);
#2673=FACE_OUTER_BOUND('',#3635,.T.);
#2674=FACE_OUTER_BOUND('',#3636,.T.);
#2675=FACE_OUTER_BOUND('',#3637,.T.);
#2676=FACE_OUTER_BOUND('',#3638,.T.);
#2677=FACE_OUTER_BOUND('',#3639,.T.);
#2678=FACE_OUTER_BOUND('',#3640,.T.);
#2679=FACE_OUTER_BOUND('',#3641,.T.);
#2680=FACE_OUTER_BOUND('',#3642,.T.);
#2681=FACE_OUTER_BOUND('',#3643,.T.);
#2682=FACE_OUTER_BOUND('',#3644,.T.);
#2683=FACE_OUTER_BOUND('',#3645,.T.);
#2684=FACE_OUTER_BOUND('',#3646,.T.);
#2685=FACE_OUTER_BOUND('',#3647,.T.);
#2686=FACE_OUTER_BOUND('',#3648,.T.);
#2687=FACE_OUTER_BOUND('',#3649,.T.);
#2688=FACE_OUTER_BOUND('',#3650,.T.);
#2689=FACE_OUTER_BOUND('',#3652,.T.);
#2690=FACE_OUTER_BOUND('',#3653,.T.);
#2691=EDGE_LOOP('',(#10019,#10020,#10021,#10022,#10023,#10024));
#2692=EDGE_LOOP('',(#10025,#10026,#10027,#10028,#10029));
#2693=EDGE_LOOP('',(#10030,#10031,#10032,#10033,#10034,#10035));
#2694=EDGE_LOOP('',(#10036,#10037,#10038,#10039));
#2695=EDGE_LOOP('',(#10040,#10041,#10042,#10043,#10044,#10045));
#2696=EDGE_LOOP('',(#10046,#10047,#10048,#10049,#10050));
#2697=EDGE_LOOP('',(#10051,#10052,#10053,#10054,#10055,#10056));
#2698=EDGE_LOOP('',(#10057,#10058,#10059,#10060));
#2699=EDGE_LOOP('',(#10061,#10062,#10063,#10064,#10065));
#2700=EDGE_LOOP('',(#10066,#10067,#10068,#10069,#10070));
#2701=EDGE_LOOP('',(#10071,#10072,#10073,#10074,#10075,#10076));
#2702=EDGE_LOOP('',(#10077,#10078,#10079,#10080,#10081));
#2703=EDGE_LOOP('',(#10082,#10083,#10084,#10085));
#2704=EDGE_LOOP('',(#10086,#10087,#10088,#10089,#10090));
#2705=EDGE_LOOP('',(#10091,#10092,#10093,#10094,#10095,#10096));
#2706=EDGE_LOOP('',(#10097,#10098,#10099,#10100,#10101,#10102));
#2707=EDGE_LOOP('',(#10103,#10104,#10105,#10106));
#2708=EDGE_LOOP('',(#10107,#10108,#10109,#10110,#10111,#10112));
#2709=EDGE_LOOP('',(#10113,#10114,#10115,#10116,#10117,#10118));
#2710=EDGE_LOOP('',(#10119,#10120,#10121,#10122));
#2711=EDGE_LOOP('',(#10123,#10124,#10125,#10126));
#2712=EDGE_LOOP('',(#10127));
#2713=EDGE_LOOP('',(#10128));
#2714=EDGE_LOOP('',(#10129,#10130,#10131,#10132));
#2715=EDGE_LOOP('',(#10133,#10134,#10135,#10136));
#2716=EDGE_LOOP('',(#10137));
#2717=EDGE_LOOP('',(#10138,#10139,#10140,#10141,#10142));
#2718=EDGE_LOOP('',(#10143,#10144,#10145,#10146,#10147,#10148));
#2719=EDGE_LOOP('',(#10149,#10150,#10151,#10152,#10153,#10154));
#2720=EDGE_LOOP('',(#10155,#10156,#10157,#10158));
#2721=EDGE_LOOP('',(#10159,#10160,#10161,#10162,#10163,#10164));
#2722=EDGE_LOOP('',(#10165,#10166,#10167,#10168,#10169));
#2723=EDGE_LOOP('',(#10170,#10171,#10172,#10173,#10174,#10175));
#2724=EDGE_LOOP('',(#10176,#10177,#10178,#10179,#10180));
#2725=EDGE_LOOP('',(#10181,#10182,#10183,#10184));
#2726=EDGE_LOOP('',(#10185,#10186,#10187,#10188,#10189));
#2727=EDGE_LOOP('',(#10190,#10191,#10192,#10193));
#2728=EDGE_LOOP('',(#10194,#10195,#10196,#10197));
#2729=EDGE_LOOP('',(#10198,#10199,#10200,#10201));
#2730=EDGE_LOOP('',(#10202,#10203,#10204,#10205,#10206,#10207));
#2731=EDGE_LOOP('',(#10208,#10209,#10210,#10211));
#2732=EDGE_LOOP('',(#10212,#10213,#10214,#10215));
#2733=EDGE_LOOP('',(#10216,#10217,#10218,#10219));
#2734=EDGE_LOOP('',(#10220,#10221,#10222,#10223));
#2735=EDGE_LOOP('',(#10224,#10225,#10226,#10227));
#2736=EDGE_LOOP('',(#10228,#10229,#10230,#10231));
#2737=EDGE_LOOP('',(#10232,#10233,#10234,#10235));
#2738=EDGE_LOOP('',(#10236,#10237,#10238,#10239));
#2739=EDGE_LOOP('',(#10240,#10241,#10242,#10243));
#2740=EDGE_LOOP('',(#10244,#10245,#10246,#10247));
#2741=EDGE_LOOP('',(#10248,#10249,#10250,#10251));
#2742=EDGE_LOOP('',(#10252,#10253,#10254,#10255));
#2743=EDGE_LOOP('',(#10256,#10257,#10258,#10259));
#2744=EDGE_LOOP('',(#10260,#10261,#10262,#10263));
#2745=EDGE_LOOP('',(#10264,#10265,#10266,#10267));
#2746=EDGE_LOOP('',(#10268,#10269,#10270,#10271));
#2747=EDGE_LOOP('',(#10272,#10273,#10274,#10275));
#2748=EDGE_LOOP('',(#10276,#10277,#10278,#10279));
#2749=EDGE_LOOP('',(#10280,#10281,#10282,#10283));
#2750=EDGE_LOOP('',(#10284,#10285,#10286,#10287));
#2751=EDGE_LOOP('',(#10288,#10289,#10290,#10291));
#2752=EDGE_LOOP('',(#10292,#10293,#10294,#10295));
#2753=EDGE_LOOP('',(#10296,#10297,#10298,#10299));
#2754=EDGE_LOOP('',(#10300,#10301,#10302,#10303));
#2755=EDGE_LOOP('',(#10304,#10305,#10306,#10307));
#2756=EDGE_LOOP('',(#10308,#10309,#10310,#10311));
#2757=EDGE_LOOP('',(#10312,#10313,#10314,#10315));
#2758=EDGE_LOOP('',(#10316,#10317,#10318,#10319));
#2759=EDGE_LOOP('',(#10320,#10321,#10322,#10323));
#2760=EDGE_LOOP('',(#10324,#10325,#10326,#10327));
#2761=EDGE_LOOP('',(#10328,#10329,#10330,#10331));
#2762=EDGE_LOOP('',(#10332,#10333,#10334,#10335));
#2763=EDGE_LOOP('',(#10336,#10337,#10338,#10339));
#2764=EDGE_LOOP('',(#10340,#10341,#10342,#10343));
#2765=EDGE_LOOP('',(#10344,#10345,#10346,#10347,#10348,#10349,#10350,#10351,
#10352,#10353,#10354,#10355,#10356,#10357,#10358,#10359,#10360,#10361,#10362,
#10363,#10364,#10365,#10366,#10367));
#2766=EDGE_LOOP('',(#10368));
#2767=EDGE_LOOP('',(#10369,#10370,#10371,#10372,#10373));
#2768=EDGE_LOOP('',(#10374,#10375,#10376,#10377,#10378));
#2769=EDGE_LOOP('',(#10379));
#2770=EDGE_LOOP('',(#10380,#10381,#10382,#10383));
#2771=EDGE_LOOP('',(#10384,#10385,#10386,#10387));
#2772=EDGE_LOOP('',(#10388,#10389,#10390,#10391,#10392));
#2773=EDGE_LOOP('',(#10393));
#2774=EDGE_LOOP('',(#10394,#10395,#10396,#10397,#10398));
#2775=EDGE_LOOP('',(#10399,#10400,#10401,#10402,#10403,#10404));
#2776=EDGE_LOOP('',(#10405,#10406,#10407,#10408));
#2777=EDGE_LOOP('',(#10409,#10410,#10411,#10412));
#2778=EDGE_LOOP('',(#10413,#10414,#10415,#10416));
#2779=EDGE_LOOP('',(#10417,#10418,#10419,#10420,#10421));
#2780=EDGE_LOOP('',(#10422,#10423,#10424,#10425,#10426));
#2781=EDGE_LOOP('',(#10427,#10428,#10429,#10430));
#2782=EDGE_LOOP('',(#10431,#10432,#10433,#10434,#10435));
#2783=EDGE_LOOP('',(#10436,#10437,#10438,#10439,#10440));
#2784=EDGE_LOOP('',(#10441,#10442,#10443,#10444));
#2785=EDGE_LOOP('',(#10445,#10446,#10447,#10448,#10449));
#2786=EDGE_LOOP('',(#10450,#10451,#10452,#10453,#10454));
#2787=EDGE_LOOP('',(#10455,#10456,#10457,#10458));
#2788=EDGE_LOOP('',(#10459,#10460,#10461,#10462,#10463));
#2789=EDGE_LOOP('',(#10464,#10465,#10466,#10467,#10468));
#2790=EDGE_LOOP('',(#10469,#10470,#10471,#10472));
#2791=EDGE_LOOP('',(#10473,#10474,#10475,#10476,#10477));
#2792=EDGE_LOOP('',(#10478,#10479,#10480,#10481));
#2793=EDGE_LOOP('',(#10482,#10483,#10484,#10485));
#2794=EDGE_LOOP('',(#10486,#10487,#10488,#10489));
#2795=EDGE_LOOP('',(#10490,#10491,#10492,#10493));
#2796=EDGE_LOOP('',(#10494,#10495,#10496,#10497));
#2797=EDGE_LOOP('',(#10498,#10499,#10500,#10501));
#2798=EDGE_LOOP('',(#10502,#10503,#10504,#10505));
#2799=EDGE_LOOP('',(#10506,#10507,#10508,#10509));
#2800=EDGE_LOOP('',(#10510,#10511,#10512,#10513,#10514,#10515,#10516,#10517,
#10518,#10519,#10520,#10521,#10522,#10523,#10524,#10525,#10526,#10527,#10528,
#10529,#10530,#10531,#10532,#10533));
#2801=EDGE_LOOP('',(#10534,#10535,#10536,#10537));
#2802=EDGE_LOOP('',(#10538,#10539,#10540,#10541));
#2803=EDGE_LOOP('',(#10542,#10543,#10544,#10545));
#2804=EDGE_LOOP('',(#10546,#10547,#10548,#10549,#10550));
#2805=EDGE_LOOP('',(#10551,#10552,#10553,#10554));
#2806=EDGE_LOOP('',(#10555,#10556,#10557,#10558,#10559));
#2807=EDGE_LOOP('',(#10560,#10561,#10562,#10563));
#2808=EDGE_LOOP('',(#10564,#10565,#10566,#10567));
#2809=EDGE_LOOP('',(#10568,#10569,#10570,#10571,#10572));
#2810=EDGE_LOOP('',(#10573,#10574,#10575,#10576));
#2811=EDGE_LOOP('',(#10577,#10578,#10579,#10580));
#2812=EDGE_LOOP('',(#10581,#10582,#10583,#10584));
#2813=EDGE_LOOP('',(#10585,#10586,#10587,#10588));
#2814=EDGE_LOOP('',(#10589,#10590,#10591,#10592));
#2815=EDGE_LOOP('',(#10593,#10594,#10595,#10596));
#2816=EDGE_LOOP('',(#10597,#10598,#10599,#10600));
#2817=EDGE_LOOP('',(#10601,#10602,#10603,#10604));
#2818=EDGE_LOOP('',(#10605,#10606,#10607,#10608));
#2819=EDGE_LOOP('',(#10609));
#2820=EDGE_LOOP('',(#10610));
#2821=EDGE_LOOP('',(#10611,#10612,#10613,#10614));
#2822=EDGE_LOOP('',(#10615,#10616,#10617,#10618,#10619,#10620,#10621,#10622,
#10623));
#2823=EDGE_LOOP('',(#10624,#10625,#10626,#10627));
#2824=EDGE_LOOP('',(#10628));
#2825=EDGE_LOOP('',(#10629));
#2826=EDGE_LOOP('',(#10630,#10631,#10632,#10633,#10634));
#2827=EDGE_LOOP('',(#10635,#10636));
#2828=EDGE_LOOP('',(#10637,#10638));
#2829=EDGE_LOOP('',(#10639,#10640,#10641,#10642,#10643,#10644));
#2830=EDGE_LOOP('',(#10645,#10646));
#2831=EDGE_LOOP('',(#10647,#10648,#10649,#10650,#10651,#10652,#10653,#10654));
#2832=EDGE_LOOP('',(#10655,#10656));
#2833=EDGE_LOOP('',(#10657));
#2834=EDGE_LOOP('',(#10658,#10659,#10660,#10661));
#2835=EDGE_LOOP('',(#10662,#10663,#10664,#10665));
#2836=EDGE_LOOP('',(#10666));
#2837=EDGE_LOOP('',(#10667));
#2838=EDGE_LOOP('',(#10668,#10669,#10670,#10671));
#2839=EDGE_LOOP('',(#10672,#10673,#10674,#10675,#10676,#10677,#10678,#10679,
#10680));
#2840=EDGE_LOOP('',(#10681,#10682));
#2841=EDGE_LOOP('',(#10683,#10684,#10685,#10686));
#2842=EDGE_LOOP('',(#10687));
#2843=EDGE_LOOP('',(#10688));
#2844=EDGE_LOOP('',(#10689,#10690,#10691,#10692));
#2845=EDGE_LOOP('',(#10693,#10694,#10695,#10696,#10697,#10698,#10699,#10700,
#10701,#10702,#10703,#10704));
#2846=EDGE_LOOP('',(#10705,#10706,#10707,#10708,#10709));
#2847=EDGE_LOOP('',(#10710));
#2848=EDGE_LOOP('',(#10711,#10712,#10713,#10714,#10715));
#2849=EDGE_LOOP('',(#10716,#10717,#10718,#10719,#10720,#10721));
#2850=EDGE_LOOP('',(#10722));
#2851=EDGE_LOOP('',(#10723,#10724,#10725,#10726,#10727,#10728));
#2852=EDGE_LOOP('',(#10729,#10730,#10731,#10732,#10733,#10734));
#2853=EDGE_LOOP('',(#10735,#10736,#10737,#10738,#10739,#10740));
#2854=EDGE_LOOP('',(#10741,#10742,#10743,#10744,#10745,#10746));
#2855=EDGE_LOOP('',(#10747,#10748,#10749,#10750,#10751));
#2856=EDGE_LOOP('',(#10752));
#2857=EDGE_LOOP('',(#10753,#10754,#10755,#10756,#10757,#10758));
#2858=EDGE_LOOP('',(#10759,#10760,#10761,#10762,#10763,#10764));
#2859=EDGE_LOOP('',(#10765,#10766,#10767,#10768,#10769,#10770,#10771,#10772,
#10773));
#2860=EDGE_LOOP('',(#10774,#10775,#10776,#10777));
#2861=EDGE_LOOP('',(#10778,#10779,#10780,#10781,#10782,#10783));
#2862=EDGE_LOOP('',(#10784,#10785,#10786,#10787));
#2863=EDGE_LOOP('',(#10788,#10789,#10790,#10791,#10792,#10793,#10794,#10795,
#10796));
#2864=EDGE_LOOP('',(#10797,#10798,#10799,#10800,#10801,#10802));
#2865=EDGE_LOOP('',(#10803,#10804,#10805,#10806,#10807,#10808,#10809,#10810));
#2866=EDGE_LOOP('',(#10811,#10812,#10813,#10814,#10815,#10816));
#2867=EDGE_LOOP('',(#10817,#10818,#10819,#10820,#10821,#10822));
#2868=EDGE_LOOP('',(#10823,#10824,#10825,#10826));
#2869=EDGE_LOOP('',(#10827,#10828,#10829,#10830,#10831,#10832));
#2870=EDGE_LOOP('',(#10833,#10834,#10835,#10836));
#2871=EDGE_LOOP('',(#10837,#10838,#10839,#10840,#10841,#10842,#10843,#10844,
#10845));
#2872=EDGE_LOOP('',(#10846,#10847,#10848,#10849,#10850,#10851));
#2873=EDGE_LOOP('',(#10852,#10853,#10854,#10855,#10856,#10857));
#2874=EDGE_LOOP('',(#10858,#10859,#10860,#10861));
#2875=EDGE_LOOP('',(#10862,#10863,#10864,#10865,#10866,#10867));
#2876=EDGE_LOOP('',(#10868,#10869,#10870,#10871,#10872,#10873));
#2877=EDGE_LOOP('',(#10874,#10875,#10876,#10877,#10878,#10879,#10880,#10881));
#2878=EDGE_LOOP('',(#10882,#10883,#10884,#10885,#10886,#10887,#10888,#10889,
#10890));
#2879=EDGE_LOOP('',(#10891,#10892,#10893,#10894));
#2880=EDGE_LOOP('',(#10895,#10896,#10897,#10898,#10899,#10900,#10901,#10902));
#2881=EDGE_LOOP('',(#10903,#10904,#10905,#10906,#10907,#10908));
#2882=EDGE_LOOP('',(#10909,#10910,#10911,#10912,#10913,#10914));
#2883=EDGE_LOOP('',(#10915,#10916,#10917,#10918));
#2884=EDGE_LOOP('',(#10919,#10920,#10921,#10922,#10923,#10924));
#2885=EDGE_LOOP('',(#10925,#10926,#10927,#10928,#10929,#10930));
#2886=EDGE_LOOP('',(#10931,#10932,#10933,#10934));
#2887=EDGE_LOOP('',(#10935,#10936,#10937,#10938,#10939,#10940));
#2888=EDGE_LOOP('',(#10941,#10942,#10943,#10944,#10945,#10946));
#2889=EDGE_LOOP('',(#10947,#10948,#10949,#10950));
#2890=EDGE_LOOP('',(#10951,#10952,#10953,#10954,#10955,#10956));
#2891=EDGE_LOOP('',(#10957,#10958,#10959,#10960));
#2892=EDGE_LOOP('',(#10961));
#2893=EDGE_LOOP('',(#10962));
#2894=EDGE_LOOP('',(#10963));
#2895=EDGE_LOOP('',(#10964));
#2896=EDGE_LOOP('',(#10965));
#2897=EDGE_LOOP('',(#10966));
#2898=EDGE_LOOP('',(#10967,#10968,#10969,#10970,#10971,#10972));
#2899=EDGE_LOOP('',(#10973,#10974,#10975,#10976));
#2900=EDGE_LOOP('',(#10977,#10978,#10979,#10980,#10981,#10982));
#2901=EDGE_LOOP('',(#10983,#10984,#10985,#10986));
#2902=EDGE_LOOP('',(#10987,#10988,#10989,#10990,#10991,#10992,#10993,#10994));
#2903=EDGE_LOOP('',(#10995,#10996,#10997,#10998,#10999,#11000));
#2904=EDGE_LOOP('',(#11001,#11002,#11003,#11004,#11005,#11006));
#2905=EDGE_LOOP('',(#11007,#11008,#11009,#11010,#11011));
#2906=EDGE_LOOP('',(#11012,#11013,#11014,#11015,#11016));
#2907=EDGE_LOOP('',(#11017));
#2908=EDGE_LOOP('',(#11018));
#2909=EDGE_LOOP('',(#11019,#11020,#11021,#11022,#11023));
#2910=EDGE_LOOP('',(#11024));
#2911=EDGE_LOOP('',(#11025));
#2912=EDGE_LOOP('',(#11026,#11027,#11028,#11029,#11030));
#2913=EDGE_LOOP('',(#11031,#11032,#11033,#11034));
#2914=EDGE_LOOP('',(#11035,#11036,#11037,#11038));
#2915=EDGE_LOOP('',(#11039,#11040,#11041,#11042));
#2916=EDGE_LOOP('',(#11043,#11044,#11045,#11046,#11047));
#2917=EDGE_LOOP('',(#11048,#11049,#11050,#11051,#11052));
#2918=EDGE_LOOP('',(#11053));
#2919=EDGE_LOOP('',(#11054));
#2920=EDGE_LOOP('',(#11055,#11056,#11057,#11058));
#2921=EDGE_LOOP('',(#11059,#11060,#11061,#11062,#11063));
#2922=EDGE_LOOP('',(#11064,#11065,#11066,#11067,#11068));
#2923=EDGE_LOOP('',(#11069));
#2924=EDGE_LOOP('',(#11070));
#2925=EDGE_LOOP('',(#11071,#11072,#11073,#11074));
#2926=EDGE_LOOP('',(#11075,#11076,#11077,#11078));
#2927=EDGE_LOOP('',(#11079,#11080,#11081,#11082));
#2928=EDGE_LOOP('',(#11083,#11084,#11085,#11086));
#2929=EDGE_LOOP('',(#11087,#11088,#11089,#11090));
#2930=EDGE_LOOP('',(#11091,#11092,#11093,#11094));
#2931=EDGE_LOOP('',(#11095,#11096,#11097,#11098));
#2932=EDGE_LOOP('',(#11099,#11100,#11101,#11102));
#2933=EDGE_LOOP('',(#11103));
#2934=EDGE_LOOP('',(#11104));
#2935=EDGE_LOOP('',(#11105));
#2936=EDGE_LOOP('',(#11106));
#2937=EDGE_LOOP('',(#11107));
#2938=EDGE_LOOP('',(#11108));
#2939=EDGE_LOOP('',(#11109,#11110,#11111,#11112));
#2940=EDGE_LOOP('',(#11113,#11114,#11115,#11116));
#2941=EDGE_LOOP('',(#11117,#11118,#11119,#11120));
#2942=EDGE_LOOP('',(#11121,#11122,#11123,#11124));
#2943=EDGE_LOOP('',(#11125,#11126,#11127,#11128,#11129,#11130));
#2944=EDGE_LOOP('',(#11131,#11132,#11133,#11134,#11135,#11136));
#2945=EDGE_LOOP('',(#11137,#11138,#11139,#11140,#11141,#11142));
#2946=EDGE_LOOP('',(#11143,#11144,#11145,#11146,#11147,#11148));
#2947=EDGE_LOOP('',(#11149,#11150,#11151,#11152));
#2948=EDGE_LOOP('',(#11153,#11154,#11155,#11156));
#2949=EDGE_LOOP('',(#11157,#11158,#11159,#11160));
#2950=EDGE_LOOP('',(#11161,#11162,#11163,#11164));
#2951=EDGE_LOOP('',(#11165,#11166,#11167,#11168));
#2952=EDGE_LOOP('',(#11169,#11170,#11171,#11172));
#2953=EDGE_LOOP('',(#11173));
#2954=EDGE_LOOP('',(#11174,#11175,#11176,#11177));
#2955=EDGE_LOOP('',(#11178,#11179,#11180,#11181));
#2956=EDGE_LOOP('',(#11182,#11183,#11184,#11185));
#2957=EDGE_LOOP('',(#11186));
#2958=EDGE_LOOP('',(#11187,#11188,#11189,#11190));
#2959=EDGE_LOOP('',(#11191,#11192,#11193,#11194));
#2960=EDGE_LOOP('',(#11195,#11196,#11197,#11198));
#2961=EDGE_LOOP('',(#11199,#11200,#11201,#11202,#11203));
#2962=EDGE_LOOP('',(#11204,#11205,#11206,#11207,#11208,#11209,#11210,#11211,
#11212,#11213,#11214,#11215,#11216));
#2963=EDGE_LOOP('',(#11217,#11218,#11219));
#2964=EDGE_LOOP('',(#11220,#11221,#11222,#11223,#11224,#11225));
#2965=EDGE_LOOP('',(#11226,#11227,#11228));
#2966=EDGE_LOOP('',(#11229,#11230,#11231,#11232,#11233,#11234,#11235,#11236));
#2967=EDGE_LOOP('',(#11237,#11238,#11239,#11240,#11241));
#2968=EDGE_LOOP('',(#11242,#11243,#11244));
#2969=EDGE_LOOP('',(#11245,#11246,#11247,#11248,#11249,#11250));
#2970=EDGE_LOOP('',(#11251,#11252,#11253,#11254));
#2971=EDGE_LOOP('',(#11255,#11256,#11257,#11258,#11259));
#2972=EDGE_LOOP('',(#11260,#11261,#11262));
#2973=EDGE_LOOP('',(#11263,#11264,#11265,#11266,#11267,#11268,#11269,#11270,
#11271));
#2974=EDGE_LOOP('',(#11272,#11273,#11274,#11275,#11276,#11277,#11278,#11279,
#11280));
#2975=EDGE_LOOP('',(#11281,#11282,#11283,#11284));
#2976=EDGE_LOOP('',(#11285,#11286,#11287,#11288));
#2977=EDGE_LOOP('',(#11289,#11290,#11291,#11292,#11293,#11294,#11295));
#2978=EDGE_LOOP('',(#11296,#11297,#11298,#11299,#11300,#11301,#11302,#11303,
#11304,#11305));
#2979=EDGE_LOOP('',(#11306,#11307,#11308,#11309));
#2980=EDGE_LOOP('',(#11310,#11311,#11312,#11313,#11314,#11315,#11316,#11317,
#11318));
#2981=EDGE_LOOP('',(#11319,#11320,#11321,#11322,#11323,#11324,#11325,#11326,
#11327,#11328,#11329,#11330));
#2982=EDGE_LOOP('',(#11331,#11332,#11333,#11334,#11335,#11336));
#2983=EDGE_LOOP('',(#11337,#11338,#11339,#11340));
#2984=EDGE_LOOP('',(#11341,#11342,#11343,#11344));
#2985=EDGE_LOOP('',(#11345,#11346,#11347,#11348));
#2986=EDGE_LOOP('',(#11349,#11350,#11351,#11352));
#2987=EDGE_LOOP('',(#11353,#11354,#11355,#11356));
#2988=EDGE_LOOP('',(#11357,#11358,#11359,#11360,#11361,#11362));
#2989=EDGE_LOOP('',(#11363));
#2990=EDGE_LOOP('',(#11364));
#2991=EDGE_LOOP('',(#11365,#11366,#11367,#11368));
#2992=EDGE_LOOP('',(#11369,#11370,#11371,#11372));
#2993=EDGE_LOOP('',(#11373,#11374,#11375,#11376));
#2994=EDGE_LOOP('',(#11377,#11378,#11379,#11380));
#2995=EDGE_LOOP('',(#11381,#11382,#11383,#11384));
#2996=EDGE_LOOP('',(#11385,#11386,#11387,#11388));
#2997=EDGE_LOOP('',(#11389,#11390,#11391,#11392));
#2998=EDGE_LOOP('',(#11393,#11394,#11395,#11396));
#2999=EDGE_LOOP('',(#11397,#11398,#11399,#11400));
#3000=EDGE_LOOP('',(#11401,#11402,#11403,#11404));
#3001=EDGE_LOOP('',(#11405,#11406,#11407,#11408));
#3002=EDGE_LOOP('',(#11409,#11410,#11411,#11412));
#3003=EDGE_LOOP('',(#11413,#11414,#11415,#11416,#11417));
#3004=EDGE_LOOP('',(#11418,#11419,#11420,#11421,#11422,#11423,#11424,#11425,
#11426,#11427,#11428,#11429,#11430,#11431,#11432,#11433));
#3005=EDGE_LOOP('',(#11434,#11435,#11436,#11437,#11438));
#3006=EDGE_LOOP('',(#11439,#11440,#11441,#11442));
#3007=EDGE_LOOP('',(#11443,#11444,#11445,#11446,#11447,#11448,#11449,#11450,
#11451,#11452,#11453,#11454,#11455,#11456,#11457,#11458));
#3008=EDGE_LOOP('',(#11459,#11460));
#3009=EDGE_LOOP('',(#11461,#11462));
#3010=EDGE_LOOP('',(#11463,#11464));
#3011=EDGE_LOOP('',(#11465,#11466));
#3012=EDGE_LOOP('',(#11467,#11468));
#3013=EDGE_LOOP('',(#11469,#11470));
#3014=EDGE_LOOP('',(#11471,#11472,#11473,#11474,#11475,#11476,#11477,#11478,
#11479,#11480,#11481,#11482,#11483,#11484,#11485,#11486,#11487,#11488,#11489,
#11490,#11491,#11492,#11493,#11494,#11495,#11496,#11497));
#3015=EDGE_LOOP('',(#11498,#11499,#11500,#11501));
#3016=EDGE_LOOP('',(#11502,#11503,#11504));
#3017=EDGE_LOOP('',(#11505,#11506,#11507,#11508));
#3018=EDGE_LOOP('',(#11509,#11510,#11511));
#3019=EDGE_LOOP('',(#11512,#11513,#11514));
#3020=EDGE_LOOP('',(#11515,#11516,#11517,#11518));
#3021=EDGE_LOOP('',(#11519,#11520,#11521));
#3022=EDGE_LOOP('',(#11522,#11523,#11524,#11525));
#3023=EDGE_LOOP('',(#11526,#11527,#11528));
#3024=EDGE_LOOP('',(#11529,#11530,#11531));
#3025=EDGE_LOOP('',(#11532,#11533,#11534));
#3026=EDGE_LOOP('',(#11535,#11536,#11537));
#3027=EDGE_LOOP('',(#11538,#11539,#11540));
#3028=EDGE_LOOP('',(#11541,#11542,#11543));
#3029=EDGE_LOOP('',(#11544,#11545,#11546));
#3030=EDGE_LOOP('',(#11547,#11548,#11549,#11550));
#3031=EDGE_LOOP('',(#11551,#11552,#11553,#11554));
#3032=EDGE_LOOP('',(#11555,#11556,#11557));
#3033=EDGE_LOOP('',(#11558,#11559,#11560));
#3034=EDGE_LOOP('',(#11561,#11562,#11563));
#3035=EDGE_LOOP('',(#11564,#11565,#11566,#11567));
#3036=EDGE_LOOP('',(#11568,#11569,#11570));
#3037=EDGE_LOOP('',(#11571,#11572,#11573));
#3038=EDGE_LOOP('',(#11574,#11575,#11576));
#3039=EDGE_LOOP('',(#11577));
#3040=EDGE_LOOP('',(#11578,#11579,#11580,#11581,#11582,#11583));
#3041=EDGE_LOOP('',(#11584,#11585,#11586,#11587));
#3042=EDGE_LOOP('',(#11588,#11589,#11590,#11591,#11592,#11593));
#3043=EDGE_LOOP('',(#11594));
#3044=EDGE_LOOP('',(#11595,#11596,#11597,#11598,#11599,#11600));
#3045=EDGE_LOOP('',(#11601,#11602,#11603,#11604));
#3046=EDGE_LOOP('',(#11605,#11606,#11607,#11608));
#3047=EDGE_LOOP('',(#11609,#11610,#11611,#11612));
#3048=EDGE_LOOP('',(#11613,#11614,#11615,#11616));
#3049=EDGE_LOOP('',(#11617,#11618,#11619,#11620));
#3050=EDGE_LOOP('',(#11621,#11622,#11623));
#3051=EDGE_LOOP('',(#11624,#11625,#11626,#11627,#11628));
#3052=EDGE_LOOP('',(#11629,#11630,#11631,#11632));
#3053=EDGE_LOOP('',(#11633,#11634,#11635,#11636));
#3054=EDGE_LOOP('',(#11637,#11638,#11639,#11640));
#3055=EDGE_LOOP('',(#11641,#11642,#11643,#11644,#11645,#11646));
#3056=EDGE_LOOP('',(#11647,#11648,#11649,#11650,#11651,#11652,#11653,#11654,
#11655,#11656,#11657,#11658,#11659));
#3057=EDGE_LOOP('',(#11660,#11661,#11662,#11663,#11664));
#3058=EDGE_LOOP('',(#11665,#11666,#11667,#11668));
#3059=EDGE_LOOP('',(#11669,#11670,#11671,#11672,#11673,#11674,#11675,#11676,
#11677,#11678,#11679,#11680,#11681,#11682));
#3060=EDGE_LOOP('',(#11683,#11684));
#3061=EDGE_LOOP('',(#11685,#11686));
#3062=EDGE_LOOP('',(#11687,#11688));
#3063=EDGE_LOOP('',(#11689,#11690));
#3064=EDGE_LOOP('',(#11691,#11692));
#3065=EDGE_LOOP('',(#11693,#11694));
#3066=EDGE_LOOP('',(#11695,#11696,#11697,#11698,#11699,#11700,#11701,#11702,
#11703,#11704,#11705,#11706,#11707,#11708,#11709,#11710,#11711,#11712,#11713,
#11714,#11715,#11716,#11717,#11718,#11719,#11720,#11721));
#3067=EDGE_LOOP('',(#11722,#11723,#11724,#11725));
#3068=EDGE_LOOP('',(#11726,#11727,#11728));
#3069=EDGE_LOOP('',(#11729,#11730,#11731,#11732));
#3070=EDGE_LOOP('',(#11733,#11734,#11735));
#3071=EDGE_LOOP('',(#11736,#11737,#11738));
#3072=EDGE_LOOP('',(#11739,#11740,#11741,#11742));
#3073=EDGE_LOOP('',(#11743,#11744,#11745));
#3074=EDGE_LOOP('',(#11746,#11747,#11748,#11749));
#3075=EDGE_LOOP('',(#11750,#11751,#11752));
#3076=EDGE_LOOP('',(#11753,#11754,#11755));
#3077=EDGE_LOOP('',(#11756,#11757,#11758));
#3078=EDGE_LOOP('',(#11759,#11760,#11761));
#3079=EDGE_LOOP('',(#11762,#11763,#11764));
#3080=EDGE_LOOP('',(#11765,#11766,#11767));
#3081=EDGE_LOOP('',(#11768,#11769,#11770));
#3082=EDGE_LOOP('',(#11771,#11772,#11773,#11774));
#3083=EDGE_LOOP('',(#11775,#11776,#11777,#11778));
#3084=EDGE_LOOP('',(#11779,#11780,#11781));
#3085=EDGE_LOOP('',(#11782,#11783,#11784));
#3086=EDGE_LOOP('',(#11785,#11786,#11787));
#3087=EDGE_LOOP('',(#11788,#11789,#11790,#11791));
#3088=EDGE_LOOP('',(#11792,#11793,#11794));
#3089=EDGE_LOOP('',(#11795,#11796,#11797));
#3090=EDGE_LOOP('',(#11798,#11799,#11800));
#3091=EDGE_LOOP('',(#11801));
#3092=EDGE_LOOP('',(#11802,#11803,#11804,#11805,#11806,#11807));
#3093=EDGE_LOOP('',(#11808,#11809,#11810,#11811));
#3094=EDGE_LOOP('',(#11812,#11813,#11814,#11815,#11816,#11817));
#3095=EDGE_LOOP('',(#11818));
#3096=EDGE_LOOP('',(#11819,#11820,#11821,#11822,#11823,#11824));
#3097=EDGE_LOOP('',(#11825,#11826,#11827,#11828,#11829,#11830));
#3098=EDGE_LOOP('',(#11831,#11832,#11833,#11834,#11835));
#3099=EDGE_LOOP('',(#11836,#11837,#11838,#11839,#11840));
#3100=EDGE_LOOP('',(#11841,#11842,#11843,#11844));
#3101=EDGE_LOOP('',(#11845,#11846,#11847,#11848));
#3102=EDGE_LOOP('',(#11849,#11850,#11851,#11852));
#3103=EDGE_LOOP('',(#11853,#11854,#11855,#11856));
#3104=EDGE_LOOP('',(#11857,#11858,#11859,#11860,#11861,#11862,#11863));
#3105=EDGE_LOOP('',(#11864,#11865,#11866,#11867,#11868));
#3106=EDGE_LOOP('',(#11869,#11870,#11871,#11872,#11873,#11874,#11875,#11876));
#3107=EDGE_LOOP('',(#11877));
#3108=EDGE_LOOP('',(#11878,#11879,#11880,#11881,#11882,#11883));
#3109=EDGE_LOOP('',(#11884,#11885,#11886,#11887));
#3110=EDGE_LOOP('',(#11888,#11889,#11890,#11891));
#3111=EDGE_LOOP('',(#11892,#11893,#11894,#11895));
#3112=EDGE_LOOP('',(#11896,#11897,#11898,#11899,#11900,#11901,#11902));
#3113=EDGE_LOOP('',(#11903,#11904,#11905,#11906));
#3114=EDGE_LOOP('',(#11907,#11908,#11909));
#3115=EDGE_LOOP('',(#11910,#11911,#11912,#11913));
#3116=EDGE_LOOP('',(#11914));
#3117=EDGE_LOOP('',(#11915));
#3118=EDGE_LOOP('',(#11916,#11917,#11918,#11919));
#3119=EDGE_LOOP('',(#11920,#11921,#11922,#11923));
#3120=EDGE_LOOP('',(#11924,#11925,#11926,#11927));
#3121=EDGE_LOOP('',(#11928,#11929,#11930,#11931));
#3122=EDGE_LOOP('',(#11932,#11933,#11934,#11935,#11936));
#3123=EDGE_LOOP('',(#11937,#11938,#11939,#11940));
#3124=EDGE_LOOP('',(#11941,#11942,#11943,#11944,#11945,#11946));
#3125=EDGE_LOOP('',(#11947,#11948,#11949,#11950,#11951,#11952));
#3126=EDGE_LOOP('',(#11953,#11954,#11955,#11956,#11957,#11958));
#3127=EDGE_LOOP('',(#11959,#11960,#11961,#11962));
#3128=EDGE_LOOP('',(#11963,#11964,#11965,#11966));
#3129=EDGE_LOOP('',(#11967,#11968,#11969,#11970,#11971,#11972,#11973));
#3130=EDGE_LOOP('',(#11974,#11975,#11976,#11977,#11978,#11979));
#3131=EDGE_LOOP('',(#11980,#11981,#11982,#11983,#11984));
#3132=EDGE_LOOP('',(#11985,#11986,#11987,#11988));
#3133=EDGE_LOOP('',(#11989,#11990,#11991,#11992,#11993));
#3134=EDGE_LOOP('',(#11994,#11995,#11996,#11997,#11998,#11999,#12000));
#3135=EDGE_LOOP('',(#12001,#12002,#12003,#12004,#12005,#12006,#12007));
#3136=EDGE_LOOP('',(#12008,#12009,#12010,#12011,#12012));
#3137=EDGE_LOOP('',(#12013,#12014,#12015,#12016,#12017,#12018));
#3138=EDGE_LOOP('',(#12019,#12020,#12021,#12022,#12023,#12024));
#3139=EDGE_LOOP('',(#12025,#12026,#12027,#12028));
#3140=EDGE_LOOP('',(#12029,#12030,#12031,#12032));
#3141=EDGE_LOOP('',(#12033,#12034,#12035,#12036,#12037,#12038));
#3142=EDGE_LOOP('',(#12039,#12040,#12041,#12042,#12043,#12044));
#3143=EDGE_LOOP('',(#12045,#12046,#12047));
#3144=EDGE_LOOP('',(#12048,#12049,#12050,#12051,#12052,#12053));
#3145=EDGE_LOOP('',(#12054,#12055,#12056,#12057));
#3146=EDGE_LOOP('',(#12058));
#3147=EDGE_LOOP('',(#12059));
#3148=EDGE_LOOP('',(#12060));
#3149=EDGE_LOOP('',(#12061));
#3150=EDGE_LOOP('',(#12062,#12063,#12064,#12065));
#3151=EDGE_LOOP('',(#12066,#12067,#12068,#12069));
#3152=EDGE_LOOP('',(#12070,#12071,#12072));
#3153=EDGE_LOOP('',(#12073,#12074,#12075,#12076));
#3154=EDGE_LOOP('',(#12077,#12078,#12079,#12080));
#3155=EDGE_LOOP('',(#12081,#12082,#12083,#12084));
#3156=EDGE_LOOP('',(#12085,#12086,#12087,#12088));
#3157=EDGE_LOOP('',(#12089,#12090,#12091,#12092));
#3158=EDGE_LOOP('',(#12093,#12094,#12095,#12096));
#3159=EDGE_LOOP('',(#12097,#12098,#12099,#12100));
#3160=EDGE_LOOP('',(#12101,#12102,#12103,#12104,#12105,#12106,#12107));
#3161=EDGE_LOOP('',(#12108,#12109,#12110,#12111));
#3162=EDGE_LOOP('',(#12112,#12113,#12114,#12115));
#3163=EDGE_LOOP('',(#12116,#12117,#12118,#12119));
#3164=EDGE_LOOP('',(#12120,#12121,#12122,#12123));
#3165=EDGE_LOOP('',(#12124));
#3166=EDGE_LOOP('',(#12125));
#3167=EDGE_LOOP('',(#12126));
#3168=EDGE_LOOP('',(#12127,#12128,#12129,#12130));
#3169=EDGE_LOOP('',(#12131,#12132,#12133,#12134));
#3170=EDGE_LOOP('',(#12135,#12136,#12137,#12138));
#3171=EDGE_LOOP('',(#12139,#12140,#12141,#12142));
#3172=EDGE_LOOP('',(#12143,#12144,#12145,#12146));
#3173=EDGE_LOOP('',(#12147,#12148,#12149,#12150,#12151,#12152,#12153,#12154,
#12155,#12156,#12157,#12158,#12159,#12160));
#3174=EDGE_LOOP('',(#12161,#12162,#12163,#12164));
#3175=EDGE_LOOP('',(#12165,#12166,#12167,#12168));
#3176=EDGE_LOOP('',(#12169,#12170,#12171,#12172));
#3177=EDGE_LOOP('',(#12173,#12174,#12175,#12176));
#3178=EDGE_LOOP('',(#12177,#12178,#12179,#12180));
#3179=EDGE_LOOP('',(#12181,#12182,#12183,#12184,#12185,#12186));
#3180=EDGE_LOOP('',(#12187,#12188,#12189));
#3181=EDGE_LOOP('',(#12190,#12191,#12192,#12193));
#3182=EDGE_LOOP('',(#12194));
#3183=EDGE_LOOP('',(#12195,#12196));
#3184=EDGE_LOOP('',(#12197,#12198,#12199,#12200,#12201,#12202));
#3185=EDGE_LOOP('',(#12203,#12204,#12205,#12206,#12207,#12208));
#3186=EDGE_LOOP('',(#12209,#12210,#12211,#12212,#12213,#12214));
#3187=EDGE_LOOP('',(#12215,#12216,#12217,#12218));
#3188=EDGE_LOOP('',(#12219,#12220,#12221,#12222));
#3189=EDGE_LOOP('',(#12223,#12224,#12225,#12226));
#3190=EDGE_LOOP('',(#12227,#12228,#12229,#12230));
#3191=EDGE_LOOP('',(#12231,#12232,#12233,#12234));
#3192=EDGE_LOOP('',(#12235,#12236,#12237,#12238));
#3193=EDGE_LOOP('',(#12239,#12240,#12241,#12242));
#3194=EDGE_LOOP('',(#12243,#12244,#12245,#12246));
#3195=EDGE_LOOP('',(#12247,#12248,#12249,#12250));
#3196=EDGE_LOOP('',(#12251,#12252,#12253,#12254));
#3197=EDGE_LOOP('',(#12255,#12256,#12257,#12258));
#3198=EDGE_LOOP('',(#12259,#12260,#12261,#12262));
#3199=EDGE_LOOP('',(#12263,#12264,#12265,#12266));
#3200=EDGE_LOOP('',(#12267,#12268,#12269,#12270));
#3201=EDGE_LOOP('',(#12271,#12272,#12273,#12274));
#3202=EDGE_LOOP('',(#12275,#12276,#12277,#12278));
#3203=EDGE_LOOP('',(#12279,#12280,#12281,#12282));
#3204=EDGE_LOOP('',(#12283,#12284,#12285,#12286));
#3205=EDGE_LOOP('',(#12287,#12288,#12289,#12290));
#3206=EDGE_LOOP('',(#12291,#12292,#12293,#12294));
#3207=EDGE_LOOP('',(#12295,#12296,#12297,#12298));
#3208=EDGE_LOOP('',(#12299,#12300,#12301,#12302));
#3209=EDGE_LOOP('',(#12303,#12304,#12305,#12306));
#3210=EDGE_LOOP('',(#12307,#12308,#12309,#12310));
#3211=EDGE_LOOP('',(#12311,#12312,#12313,#12314));
#3212=EDGE_LOOP('',(#12315,#12316,#12317,#12318,#12319));
#3213=EDGE_LOOP('',(#12320,#12321,#12322,#12323));
#3214=EDGE_LOOP('',(#12324,#12325,#12326,#12327));
#3215=EDGE_LOOP('',(#12328,#12329,#12330,#12331));
#3216=EDGE_LOOP('',(#12332,#12333,#12334,#12335));
#3217=EDGE_LOOP('',(#12336,#12337,#12338,#12339));
#3218=EDGE_LOOP('',(#12340,#12341,#12342,#12343));
#3219=EDGE_LOOP('',(#12344,#12345,#12346,#12347));
#3220=EDGE_LOOP('',(#12348,#12349,#12350,#12351));
#3221=EDGE_LOOP('',(#12352,#12353,#12354,#12355));
#3222=EDGE_LOOP('',(#12356,#12357,#12358,#12359));
#3223=EDGE_LOOP('',(#12360,#12361,#12362,#12363));
#3224=EDGE_LOOP('',(#12364,#12365,#12366,#12367));
#3225=EDGE_LOOP('',(#12368,#12369,#12370,#12371));
#3226=EDGE_LOOP('',(#12372,#12373,#12374,#12375));
#3227=EDGE_LOOP('',(#12376,#12377,#12378,#12379));
#3228=EDGE_LOOP('',(#12380,#12381,#12382,#12383));
#3229=EDGE_LOOP('',(#12384,#12385,#12386,#12387));
#3230=EDGE_LOOP('',(#12388,#12389,#12390,#12391));
#3231=EDGE_LOOP('',(#12392,#12393,#12394,#12395));
#3232=EDGE_LOOP('',(#12396,#12397,#12398,#12399));
#3233=EDGE_LOOP('',(#12400,#12401,#12402,#12403));
#3234=EDGE_LOOP('',(#12404,#12405,#12406,#12407));
#3235=EDGE_LOOP('',(#12408,#12409,#12410,#12411));
#3236=EDGE_LOOP('',(#12412,#12413,#12414,#12415));
#3237=EDGE_LOOP('',(#12416,#12417,#12418,#12419));
#3238=EDGE_LOOP('',(#12420,#12421,#12422,#12423));
#3239=EDGE_LOOP('',(#12424,#12425,#12426,#12427));
#3240=EDGE_LOOP('',(#12428,#12429,#12430,#12431));
#3241=EDGE_LOOP('',(#12432,#12433,#12434,#12435));
#3242=EDGE_LOOP('',(#12436));
#3243=EDGE_LOOP('',(#12437,#12438,#12439,#12440,#12441,#12442,#12443,#12444,
#12445,#12446,#12447,#12448,#12449,#12450,#12451,#12452,#12453,#12454,#12455,
#12456,#12457,#12458,#12459,#12460,#12461,#12462,#12463,#12464,#12465,#12466,
#12467,#12468,#12469,#12470,#12471,#12472,#12473,#12474,#12475,#12476,#12477,
#12478,#12479,#12480,#12481,#12482,#12483,#12484,#12485,#12486,#12487));
#3244=EDGE_LOOP('',(#12488,#12489,#12490,#12491,#12492));
#3245=EDGE_LOOP('',(#12493,#12494,#12495,#12496));
#3246=EDGE_LOOP('',(#12497,#12498,#12499,#12500,#12501,#12502,#12503,#12504,
#12505,#12506,#12507,#12508,#12509,#12510,#12511,#12512,#12513,#12514,#12515,
#12516,#12517,#12518,#12519,#12520,#12521,#12522,#12523,#12524,#12525,#12526,
#12527,#12528,#12529,#12530,#12531,#12532,#12533,#12534,#12535,#12536,#12537,
#12538,#12539,#12540,#12541,#12542,#12543,#12544,#12545,#12546));
#3247=EDGE_LOOP('',(#12547,#12548,#12549,#12550));
#3248=EDGE_LOOP('',(#12551,#12552,#12553,#12554));
#3249=EDGE_LOOP('',(#12555,#12556,#12557,#12558));
#3250=EDGE_LOOP('',(#12559,#12560,#12561,#12562));
#3251=EDGE_LOOP('',(#12563,#12564,#12565,#12566));
#3252=EDGE_LOOP('',(#12567,#12568,#12569,#12570));
#3253=EDGE_LOOP('',(#12571,#12572,#12573,#12574));
#3254=EDGE_LOOP('',(#12575,#12576,#12577,#12578));
#3255=EDGE_LOOP('',(#12579,#12580,#12581,#12582));
#3256=EDGE_LOOP('',(#12583,#12584,#12585,#12586));
#3257=EDGE_LOOP('',(#12587,#12588,#12589,#12590));
#3258=EDGE_LOOP('',(#12591,#12592,#12593,#12594));
#3259=EDGE_LOOP('',(#12595,#12596,#12597,#12598));
#3260=EDGE_LOOP('',(#12599,#12600,#12601,#12602));
#3261=EDGE_LOOP('',(#12603,#12604,#12605,#12606));
#3262=EDGE_LOOP('',(#12607,#12608,#12609,#12610));
#3263=EDGE_LOOP('',(#12611,#12612,#12613,#12614));
#3264=EDGE_LOOP('',(#12615,#12616,#12617,#12618));
#3265=EDGE_LOOP('',(#12619,#12620,#12621,#12622));
#3266=EDGE_LOOP('',(#12623,#12624,#12625,#12626));
#3267=EDGE_LOOP('',(#12627,#12628,#12629,#12630));
#3268=EDGE_LOOP('',(#12631,#12632,#12633,#12634));
#3269=EDGE_LOOP('',(#12635,#12636,#12637,#12638));
#3270=EDGE_LOOP('',(#12639,#12640,#12641,#12642));
#3271=EDGE_LOOP('',(#12643,#12644,#12645,#12646));
#3272=EDGE_LOOP('',(#12647,#12648,#12649,#12650));
#3273=EDGE_LOOP('',(#12651,#12652,#12653,#12654));
#3274=EDGE_LOOP('',(#12655,#12656,#12657,#12658));
#3275=EDGE_LOOP('',(#12659,#12660,#12661,#12662));
#3276=EDGE_LOOP('',(#12663,#12664,#12665,#12666));
#3277=EDGE_LOOP('',(#12667,#12668,#12669,#12670));
#3278=EDGE_LOOP('',(#12671,#12672,#12673,#12674));
#3279=EDGE_LOOP('',(#12675,#12676,#12677,#12678));
#3280=EDGE_LOOP('',(#12679,#12680,#12681,#12682));
#3281=EDGE_LOOP('',(#12683,#12684,#12685,#12686));
#3282=EDGE_LOOP('',(#12687,#12688,#12689,#12690));
#3283=EDGE_LOOP('',(#12691,#12692,#12693,#12694));
#3284=EDGE_LOOP('',(#12695,#12696,#12697,#12698));
#3285=EDGE_LOOP('',(#12699,#12700,#12701,#12702));
#3286=EDGE_LOOP('',(#12703,#12704,#12705,#12706));
#3287=EDGE_LOOP('',(#12707,#12708,#12709,#12710));
#3288=EDGE_LOOP('',(#12711,#12712,#12713,#12714));
#3289=EDGE_LOOP('',(#12715,#12716,#12717,#12718));
#3290=EDGE_LOOP('',(#12719,#12720,#12721,#12722));
#3291=EDGE_LOOP('',(#12723,#12724,#12725,#12726));
#3292=EDGE_LOOP('',(#12727,#12728,#12729,#12730));
#3293=EDGE_LOOP('',(#12731,#12732,#12733,#12734));
#3294=EDGE_LOOP('',(#12735,#12736,#12737,#12738));
#3295=EDGE_LOOP('',(#12739,#12740,#12741,#12742));
#3296=EDGE_LOOP('',(#12743,#12744,#12745,#12746));
#3297=EDGE_LOOP('',(#12747,#12748,#12749,#12750));
#3298=EDGE_LOOP('',(#12751,#12752,#12753,#12754));
#3299=EDGE_LOOP('',(#12755,#12756,#12757,#12758));
#3300=EDGE_LOOP('',(#12759,#12760,#12761,#12762));
#3301=EDGE_LOOP('',(#12763,#12764,#12765,#12766));
#3302=EDGE_LOOP('',(#12767,#12768,#12769,#12770));
#3303=EDGE_LOOP('',(#12771,#12772,#12773,#12774));
#3304=EDGE_LOOP('',(#12775,#12776,#12777,#12778));
#3305=EDGE_LOOP('',(#12779,#12780,#12781,#12782));
#3306=EDGE_LOOP('',(#12783,#12784,#12785,#12786));
#3307=EDGE_LOOP('',(#12787,#12788,#12789,#12790));
#3308=EDGE_LOOP('',(#12791,#12792,#12793,#12794));
#3309=EDGE_LOOP('',(#12795,#12796,#12797,#12798));
#3310=EDGE_LOOP('',(#12799,#12800,#12801,#12802));
#3311=EDGE_LOOP('',(#12803,#12804,#12805,#12806));
#3312=EDGE_LOOP('',(#12807,#12808,#12809,#12810));
#3313=EDGE_LOOP('',(#12811,#12812,#12813,#12814));
#3314=EDGE_LOOP('',(#12815,#12816,#12817,#12818));
#3315=EDGE_LOOP('',(#12819,#12820,#12821,#12822));
#3316=EDGE_LOOP('',(#12823,#12824,#12825,#12826));
#3317=EDGE_LOOP('',(#12827,#12828,#12829,#12830));
#3318=EDGE_LOOP('',(#12831,#12832,#12833,#12834));
#3319=EDGE_LOOP('',(#12835,#12836,#12837,#12838));
#3320=EDGE_LOOP('',(#12839,#12840,#12841,#12842));
#3321=EDGE_LOOP('',(#12843,#12844,#12845,#12846));
#3322=EDGE_LOOP('',(#12847,#12848,#12849,#12850));
#3323=EDGE_LOOP('',(#12851,#12852,#12853,#12854));
#3324=EDGE_LOOP('',(#12855,#12856,#12857,#12858));
#3325=EDGE_LOOP('',(#12859,#12860,#12861,#12862));
#3326=EDGE_LOOP('',(#12863,#12864,#12865,#12866));
#3327=EDGE_LOOP('',(#12867,#12868,#12869,#12870));
#3328=EDGE_LOOP('',(#12871,#12872,#12873,#12874));
#3329=EDGE_LOOP('',(#12875,#12876,#12877,#12878));
#3330=EDGE_LOOP('',(#12879,#12880,#12881,#12882));
#3331=EDGE_LOOP('',(#12883,#12884,#12885,#12886));
#3332=EDGE_LOOP('',(#12887,#12888,#12889,#12890));
#3333=EDGE_LOOP('',(#12891,#12892,#12893,#12894));
#3334=EDGE_LOOP('',(#12895,#12896,#12897,#12898));
#3335=EDGE_LOOP('',(#12899,#12900,#12901,#12902));
#3336=EDGE_LOOP('',(#12903,#12904,#12905,#12906));
#3337=EDGE_LOOP('',(#12907,#12908,#12909,#12910,#12911,#12912,#12913,#12914,
#12915,#12916,#12917,#12918,#12919,#12920,#12921,#12922,#12923,#12924,#12925,
#12926,#12927,#12928,#12929,#12930,#12931,#12932,#12933,#12934,#12935,#12936,
#12937,#12938,#12939,#12940,#12941,#12942,#12943,#12944,#12945,#12946,#12947,
#12948,#12949,#12950,#12951,#12952,#12953,#12954,#12955,#12956,#12957,#12958,
#12959,#12960,#12961,#12962,#12963,#12964,#12965,#12966,#12967,#12968,#12969,
#12970,#12971,#12972,#12973,#12974,#12975,#12976,#12977,#12978,#12979,#12980,
#12981,#12982,#12983,#12984,#12985,#12986,#12987,#12988,#12989,#12990,#12991,
#12992,#12993,#12994,#12995,#12996,#12997,#12998,#12999));
#3338=EDGE_LOOP('',(#13000));
#3339=EDGE_LOOP('',(#13001));
#3340=EDGE_LOOP('',(#13002,#13003,#13004,#13005,#13006,#13007));
#3341=EDGE_LOOP('',(#13008,#13009,#13010));
#3342=EDGE_LOOP('',(#13011));
#3343=EDGE_LOOP('',(#13012,#13013,#13014,#13015,#13016));
#3344=EDGE_LOOP('',(#13017,#13018,#13019,#13020,#13021,#13022,#13023,#13024,
#13025,#13026,#13027,#13028,#13029,#13030,#13031,#13032,#13033,#13034,#13035,
#13036,#13037,#13038,#13039,#13040,#13041,#13042,#13043,#13044,#13045,#13046,
#13047,#13048,#13049,#13050,#13051,#13052,#13053,#13054,#13055,#13056,#13057,
#13058,#13059,#13060,#13061,#13062,#13063,#13064,#13065,#13066,#13067,#13068,
#13069,#13070,#13071,#13072,#13073,#13074,#13075,#13076,#13077,#13078,#13079,
#13080,#13081,#13082,#13083,#13084,#13085,#13086,#13087,#13088,#13089,#13090,
#13091,#13092,#13093,#13094,#13095,#13096,#13097,#13098,#13099,#13100,#13101,
#13102,#13103,#13104,#13105,#13106,#13107,#13108,#13109));
#3345=EDGE_LOOP('',(#13110));
#3346=EDGE_LOOP('',(#13111,#13112,#13113,#13114));
#3347=EDGE_LOOP('',(#13115,#13116));
#3348=EDGE_LOOP('',(#13117,#13118,#13119,#13120));
#3349=EDGE_LOOP('',(#13121));
#3350=EDGE_LOOP('',(#13122));
#3351=EDGE_LOOP('',(#13123,#13124,#13125,#13126));
#3352=EDGE_LOOP('',(#13127,#13128,#13129,#13130));
#3353=EDGE_LOOP('',(#13131,#13132,#13133,#13134));
#3354=EDGE_LOOP('',(#13135,#13136,#13137,#13138));
#3355=EDGE_LOOP('',(#13139,#13140,#13141,#13142));
#3356=EDGE_LOOP('',(#13143,#13144,#13145,#13146));
#3357=EDGE_LOOP('',(#13147,#13148,#13149,#13150));
#3358=EDGE_LOOP('',(#13151,#13152,#13153,#13154));
#3359=EDGE_LOOP('',(#13155,#13156,#13157,#13158));
#3360=EDGE_LOOP('',(#13159,#13160,#13161,#13162));
#3361=EDGE_LOOP('',(#13163,#13164,#13165,#13166));
#3362=EDGE_LOOP('',(#13167,#13168,#13169,#13170));
#3363=EDGE_LOOP('',(#13171,#13172,#13173,#13174));
#3364=EDGE_LOOP('',(#13175,#13176,#13177,#13178));
#3365=EDGE_LOOP('',(#13179,#13180,#13181,#13182));
#3366=EDGE_LOOP('',(#13183,#13184,#13185,#13186));
#3367=EDGE_LOOP('',(#13187,#13188,#13189,#13190));
#3368=EDGE_LOOP('',(#13191,#13192,#13193,#13194));
#3369=EDGE_LOOP('',(#13195,#13196,#13197,#13198));
#3370=EDGE_LOOP('',(#13199,#13200,#13201,#13202));
#3371=EDGE_LOOP('',(#13203,#13204,#13205,#13206));
#3372=EDGE_LOOP('',(#13207,#13208,#13209,#13210));
#3373=EDGE_LOOP('',(#13211,#13212,#13213,#13214));
#3374=EDGE_LOOP('',(#13215,#13216,#13217,#13218));
#3375=EDGE_LOOP('',(#13219,#13220,#13221,#13222));
#3376=EDGE_LOOP('',(#13223,#13224,#13225,#13226));
#3377=EDGE_LOOP('',(#13227,#13228,#13229,#13230));
#3378=EDGE_LOOP('',(#13231,#13232,#13233,#13234));
#3379=EDGE_LOOP('',(#13235,#13236,#13237,#13238));
#3380=EDGE_LOOP('',(#13239,#13240,#13241,#13242));
#3381=EDGE_LOOP('',(#13243,#13244,#13245,#13246));
#3382=EDGE_LOOP('',(#13247,#13248,#13249,#13250));
#3383=EDGE_LOOP('',(#13251,#13252,#13253,#13254));
#3384=EDGE_LOOP('',(#13255,#13256,#13257,#13258));
#3385=EDGE_LOOP('',(#13259,#13260,#13261,#13262));
#3386=EDGE_LOOP('',(#13263,#13264,#13265,#13266));
#3387=EDGE_LOOP('',(#13267,#13268,#13269,#13270));
#3388=EDGE_LOOP('',(#13271,#13272,#13273,#13274));
#3389=EDGE_LOOP('',(#13275,#13276,#13277,#13278));
#3390=EDGE_LOOP('',(#13279,#13280,#13281,#13282));
#3391=EDGE_LOOP('',(#13283,#13284,#13285,#13286));
#3392=EDGE_LOOP('',(#13287,#13288,#13289,#13290));
#3393=EDGE_LOOP('',(#13291,#13292,#13293,#13294));
#3394=EDGE_LOOP('',(#13295,#13296,#13297,#13298));
#3395=EDGE_LOOP('',(#13299,#13300,#13301,#13302,#13303));
#3396=EDGE_LOOP('',(#13304,#13305,#13306,#13307,#13308,#13309,#13310,#13311,
#13312,#13313,#13314,#13315,#13316,#13317,#13318,#13319,#13320,#13321,#13322,
#13323,#13324,#13325,#13326,#13327,#13328,#13329,#13330,#13331,#13332,#13333,
#13334,#13335,#13336,#13337,#13338,#13339,#13340,#13341,#13342,#13343,#13344,
#13345,#13346,#13347,#13348,#13349,#13350,#13351));
#3397=EDGE_LOOP('',(#13352,#13353,#13354,#13355,#13356));
#3398=EDGE_LOOP('',(#13357,#13358,#13359,#13360));
#3399=EDGE_LOOP('',(#13361,#13362,#13363,#13364,#13365,#13366,#13367,#13368,
#13369,#13370,#13371,#13372,#13373,#13374,#13375,#13376,#13377,#13378,#13379,
#13380,#13381,#13382,#13383,#13384,#13385,#13386,#13387,#13388,#13389,#13390,
#13391,#13392,#13393,#13394,#13395,#13396,#13397,#13398,#13399,#13400,#13401,
#13402,#13403,#13404,#13405,#13406,#13407,#13408));
#3400=EDGE_LOOP('',(#13409,#13410,#13411,#13412,#13413,#13414));
#3401=EDGE_LOOP('',(#13415,#13416,#13417,#13418));
#3402=EDGE_LOOP('',(#13419,#13420,#13421,#13422,#13423,#13424,#13425,#13426,
#13427,#13428,#13429,#13430,#13431,#13432,#13433,#13434,#13435,#13436,#13437,
#13438,#13439,#13440,#13441,#13442,#13443,#13444,#13445,#13446,#13447,#13448,
#13449,#13450,#13451,#13452,#13453,#13454,#13455,#13456,#13457,#13458,#13459,
#13460,#13461,#13462,#13463,#13464,#13465,#13466,#13467,#13468,#13469,#13470,
#13471,#13472,#13473,#13474,#13475,#13476,#13477,#13478,#13479,#13480,#13481,
#13482,#13483,#13484,#13485,#13486,#13487,#13488,#13489,#13490,#13491,#13492,
#13493,#13494,#13495,#13496,#13497,#13498,#13499,#13500,#13501,#13502,#13503,
#13504,#13505,#13506,#13507,#13508,#13509,#13510,#13511,#13512,#13513,#13514,
#13515,#13516,#13517,#13518,#13519,#13520,#13521,#13522,#13523,#13524,#13525,
#13526));
#3403=EDGE_LOOP('',(#13527));
#3404=EDGE_LOOP('',(#13528,#13529));
#3405=EDGE_LOOP('',(#13530,#13531));
#3406=EDGE_LOOP('',(#13532,#13533));
#3407=EDGE_LOOP('',(#13534,#13535));
#3408=EDGE_LOOP('',(#13536,#13537));
#3409=EDGE_LOOP('',(#13538,#13539));
#3410=EDGE_LOOP('',(#13540,#13541,#13542,#13543,#13544,#13545,#13546,#13547,
#13548,#13549,#13550,#13551,#13552,#13553,#13554,#13555,#13556,#13557,#13558,
#13559,#13560,#13561,#13562,#13563,#13564,#13565,#13566));
#3411=EDGE_LOOP('',(#13567,#13568,#13569,#13570));
#3412=EDGE_LOOP('',(#13571,#13572,#13573));
#3413=EDGE_LOOP('',(#13574,#13575,#13576,#13577));
#3414=EDGE_LOOP('',(#13578,#13579,#13580));
#3415=EDGE_LOOP('',(#13581,#13582,#13583));
#3416=EDGE_LOOP('',(#13584,#13585,#13586,#13587));
#3417=EDGE_LOOP('',(#13588,#13589,#13590));
#3418=EDGE_LOOP('',(#13591,#13592,#13593,#13594));
#3419=EDGE_LOOP('',(#13595,#13596,#13597));
#3420=EDGE_LOOP('',(#13598,#13599,#13600));
#3421=EDGE_LOOP('',(#13601,#13602,#13603));
#3422=EDGE_LOOP('',(#13604,#13605,#13606));
#3423=EDGE_LOOP('',(#13607,#13608,#13609));
#3424=EDGE_LOOP('',(#13610,#13611,#13612));
#3425=EDGE_LOOP('',(#13613,#13614,#13615));
#3426=EDGE_LOOP('',(#13616,#13617,#13618,#13619));
#3427=EDGE_LOOP('',(#13620,#13621,#13622,#13623));
#3428=EDGE_LOOP('',(#13624,#13625,#13626));
#3429=EDGE_LOOP('',(#13627,#13628,#13629));
#3430=EDGE_LOOP('',(#13630,#13631,#13632));
#3431=EDGE_LOOP('',(#13633,#13634,#13635,#13636));
#3432=EDGE_LOOP('',(#13637,#13638,#13639));
#3433=EDGE_LOOP('',(#13640,#13641,#13642));
#3434=EDGE_LOOP('',(#13643,#13644,#13645));
#3435=EDGE_LOOP('',(#13646,#13647,#13648,#13649));
#3436=EDGE_LOOP('',(#13650,#13651,#13652,#13653));
#3437=EDGE_LOOP('',(#13654,#13655,#13656,#13657));
#3438=EDGE_LOOP('',(#13658,#13659,#13660,#13661));
#3439=EDGE_LOOP('',(#13662,#13663,#13664,#13665));
#3440=EDGE_LOOP('',(#13666,#13667,#13668,#13669));
#3441=EDGE_LOOP('',(#13670,#13671,#13672,#13673));
#3442=EDGE_LOOP('',(#13674,#13675,#13676,#13677));
#3443=EDGE_LOOP('',(#13678,#13679,#13680,#13681));
#3444=EDGE_LOOP('',(#13682,#13683,#13684,#13685));
#3445=EDGE_LOOP('',(#13686,#13687,#13688,#13689));
#3446=EDGE_LOOP('',(#13690,#13691,#13692,#13693));
#3447=EDGE_LOOP('',(#13694,#13695,#13696,#13697));
#3448=EDGE_LOOP('',(#13698,#13699,#13700,#13701));
#3449=EDGE_LOOP('',(#13702,#13703,#13704,#13705));
#3450=EDGE_LOOP('',(#13706,#13707,#13708,#13709));
#3451=EDGE_LOOP('',(#13710,#13711,#13712,#13713));
#3452=EDGE_LOOP('',(#13714,#13715,#13716,#13717));
#3453=EDGE_LOOP('',(#13718,#13719,#13720,#13721));
#3454=EDGE_LOOP('',(#13722,#13723,#13724,#13725));
#3455=EDGE_LOOP('',(#13726,#13727,#13728,#13729));
#3456=EDGE_LOOP('',(#13730,#13731,#13732,#13733));
#3457=EDGE_LOOP('',(#13734,#13735,#13736,#13737));
#3458=EDGE_LOOP('',(#13738,#13739,#13740,#13741));
#3459=EDGE_LOOP('',(#13742,#13743,#13744,#13745));
#3460=EDGE_LOOP('',(#13746,#13747,#13748,#13749));
#3461=EDGE_LOOP('',(#13750,#13751,#13752,#13753));
#3462=EDGE_LOOP('',(#13754,#13755,#13756,#13757));
#3463=EDGE_LOOP('',(#13758,#13759,#13760,#13761));
#3464=EDGE_LOOP('',(#13762,#13763,#13764,#13765));
#3465=EDGE_LOOP('',(#13766,#13767,#13768,#13769));
#3466=EDGE_LOOP('',(#13770,#13771,#13772,#13773));
#3467=EDGE_LOOP('',(#13774,#13775,#13776,#13777));
#3468=EDGE_LOOP('',(#13778,#13779,#13780,#13781));
#3469=EDGE_LOOP('',(#13782,#13783,#13784,#13785));
#3470=EDGE_LOOP('',(#13786,#13787,#13788,#13789));
#3471=EDGE_LOOP('',(#13790,#13791,#13792,#13793));
#3472=EDGE_LOOP('',(#13794,#13795,#13796,#13797));
#3473=EDGE_LOOP('',(#13798,#13799,#13800,#13801));
#3474=EDGE_LOOP('',(#13802,#13803,#13804,#13805));
#3475=EDGE_LOOP('',(#13806,#13807,#13808,#13809));
#3476=EDGE_LOOP('',(#13810,#13811,#13812,#13813));
#3477=EDGE_LOOP('',(#13814,#13815,#13816,#13817));
#3478=EDGE_LOOP('',(#13818,#13819,#13820,#13821));
#3479=EDGE_LOOP('',(#13822,#13823,#13824,#13825));
#3480=EDGE_LOOP('',(#13826,#13827,#13828,#13829));
#3481=EDGE_LOOP('',(#13830,#13831,#13832,#13833));
#3482=EDGE_LOOP('',(#13834,#13835,#13836,#13837));
#3483=EDGE_LOOP('',(#13838,#13839,#13840,#13841));
#3484=EDGE_LOOP('',(#13842,#13843,#13844,#13845));
#3485=EDGE_LOOP('',(#13846,#13847,#13848,#13849));
#3486=EDGE_LOOP('',(#13850,#13851,#13852,#13853));
#3487=EDGE_LOOP('',(#13854,#13855,#13856,#13857));
#3488=EDGE_LOOP('',(#13858,#13859,#13860,#13861));
#3489=EDGE_LOOP('',(#13862,#13863,#13864,#13865));
#3490=EDGE_LOOP('',(#13866,#13867,#13868,#13869));
#3491=EDGE_LOOP('',(#13870,#13871,#13872,#13873));
#3492=EDGE_LOOP('',(#13874,#13875,#13876,#13877));
#3493=EDGE_LOOP('',(#13878,#13879,#13880,#13881));
#3494=EDGE_LOOP('',(#13882,#13883,#13884,#13885));
#3495=EDGE_LOOP('',(#13886,#13887,#13888,#13889));
#3496=EDGE_LOOP('',(#13890,#13891,#13892,#13893));
#3497=EDGE_LOOP('',(#13894,#13895,#13896,#13897));
#3498=EDGE_LOOP('',(#13898,#13899,#13900,#13901));
#3499=EDGE_LOOP('',(#13902,#13903,#13904,#13905));
#3500=EDGE_LOOP('',(#13906,#13907,#13908,#13909));
#3501=EDGE_LOOP('',(#13910,#13911,#13912,#13913));
#3502=EDGE_LOOP('',(#13914,#13915,#13916,#13917));
#3503=EDGE_LOOP('',(#13918,#13919,#13920,#13921));
#3504=EDGE_LOOP('',(#13922,#13923,#13924,#13925));
#3505=EDGE_LOOP('',(#13926,#13927,#13928,#13929));
#3506=EDGE_LOOP('',(#13930,#13931,#13932,#13933));
#3507=EDGE_LOOP('',(#13934,#13935,#13936,#13937));
#3508=EDGE_LOOP('',(#13938,#13939,#13940,#13941));
#3509=EDGE_LOOP('',(#13942,#13943,#13944,#13945));
#3510=EDGE_LOOP('',(#13946,#13947,#13948,#13949));
#3511=EDGE_LOOP('',(#13950,#13951,#13952,#13953));
#3512=EDGE_LOOP('',(#13954,#13955,#13956,#13957));
#3513=EDGE_LOOP('',(#13958,#13959,#13960,#13961));
#3514=EDGE_LOOP('',(#13962,#13963,#13964,#13965));
#3515=EDGE_LOOP('',(#13966,#13967,#13968,#13969));
#3516=EDGE_LOOP('',(#13970,#13971,#13972,#13973));
#3517=EDGE_LOOP('',(#13974,#13975,#13976,#13977));
#3518=EDGE_LOOP('',(#13978,#13979,#13980,#13981));
#3519=EDGE_LOOP('',(#13982,#13983,#13984,#13985));
#3520=EDGE_LOOP('',(#13986,#13987,#13988,#13989));
#3521=EDGE_LOOP('',(#13990,#13991,#13992,#13993));
#3522=EDGE_LOOP('',(#13994,#13995,#13996,#13997));
#3523=EDGE_LOOP('',(#13998,#13999,#14000,#14001));
#3524=EDGE_LOOP('',(#14002,#14003,#14004,#14005));
#3525=EDGE_LOOP('',(#14006,#14007,#14008,#14009));
#3526=EDGE_LOOP('',(#14010,#14011,#14012,#14013));
#3527=EDGE_LOOP('',(#14014,#14015,#14016,#14017));
#3528=EDGE_LOOP('',(#14018,#14019,#14020,#14021));
#3529=EDGE_LOOP('',(#14022,#14023,#14024,#14025));
#3530=EDGE_LOOP('',(#14026,#14027,#14028,#14029));
#3531=EDGE_LOOP('',(#14030,#14031,#14032,#14033));
#3532=EDGE_LOOP('',(#14034,#14035,#14036,#14037));
#3533=EDGE_LOOP('',(#14038,#14039,#14040,#14041));
#3534=EDGE_LOOP('',(#14042,#14043,#14044,#14045));
#3535=EDGE_LOOP('',(#14046,#14047,#14048,#14049));
#3536=EDGE_LOOP('',(#14050,#14051,#14052,#14053));
#3537=EDGE_LOOP('',(#14054,#14055,#14056,#14057));
#3538=EDGE_LOOP('',(#14058,#14059,#14060,#14061));
#3539=EDGE_LOOP('',(#14062,#14063,#14064,#14065));
#3540=EDGE_LOOP('',(#14066,#14067,#14068,#14069));
#3541=EDGE_LOOP('',(#14070,#14071,#14072,#14073));
#3542=EDGE_LOOP('',(#14074,#14075,#14076,#14077));
#3543=EDGE_LOOP('',(#14078));
#3544=EDGE_LOOP('',(#14079,#14080,#14081,#14082,#14083,#14084));
#3545=EDGE_LOOP('',(#14085,#14086,#14087,#14088,#14089,#14090,#14091,#14092,
#14093,#14094,#14095,#14096,#14097,#14098,#14099,#14100,#14101,#14102,#14103,
#14104,#14105,#14106,#14107,#14108,#14109,#14110,#14111,#14112,#14113,#14114,
#14115,#14116,#14117,#14118,#14119,#14120,#14121,#14122,#14123,#14124,#14125,
#14126,#14127,#14128,#14129,#14130,#14131,#14132,#14133,#14134,#14135,#14136,
#14137,#14138,#14139,#14140,#14141,#14142,#14143,#14144,#14145,#14146,#14147,
#14148,#14149,#14150,#14151,#14152,#14153,#14154,#14155,#14156,#14157,#14158,
#14159,#14160,#14161,#14162,#14163,#14164,#14165,#14166,#14167,#14168,#14169,
#14170,#14171,#14172,#14173,#14174,#14175,#14176,#14177,#14178,#14179,#14180,
#14181,#14182,#14183,#14184,#14185,#14186,#14187,#14188,#14189,#14190,#14191,
#14192,#14193,#14194,#14195));
#3546=EDGE_LOOP('',(#14196));
#3547=EDGE_LOOP('',(#14197,#14198,#14199,#14200,#14201,#14202));
#3548=EDGE_LOOP('',(#14203,#14204,#14205,#14206));
#3549=EDGE_LOOP('',(#14207,#14208,#14209,#14210));
#3550=EDGE_LOOP('',(#14211,#14212,#14213,#14214));
#3551=EDGE_LOOP('',(#14215,#14216,#14217,#14218));
#3552=EDGE_LOOP('',(#14219,#14220,#14221,#14222));
#3553=EDGE_LOOP('',(#14223,#14224,#14225,#14226));
#3554=EDGE_LOOP('',(#14227,#14228,#14229,#14230));
#3555=EDGE_LOOP('',(#14231,#14232,#14233,#14234));
#3556=EDGE_LOOP('',(#14235,#14236,#14237,#14238));
#3557=EDGE_LOOP('',(#14239,#14240,#14241,#14242));
#3558=EDGE_LOOP('',(#14243,#14244,#14245,#14246));
#3559=EDGE_LOOP('',(#14247,#14248,#14249,#14250));
#3560=EDGE_LOOP('',(#14251,#14252,#14253,#14254));
#3561=EDGE_LOOP('',(#14255,#14256,#14257,#14258));
#3562=EDGE_LOOP('',(#14259,#14260,#14261,#14262));
#3563=EDGE_LOOP('',(#14263,#14264,#14265,#14266));
#3564=EDGE_LOOP('',(#14267,#14268,#14269,#14270));
#3565=EDGE_LOOP('',(#14271,#14272,#14273,#14274));
#3566=EDGE_LOOP('',(#14275,#14276,#14277,#14278));
#3567=EDGE_LOOP('',(#14279,#14280,#14281,#14282));
#3568=EDGE_LOOP('',(#14283,#14284,#14285,#14286));
#3569=EDGE_LOOP('',(#14287,#14288,#14289,#14290));
#3570=EDGE_LOOP('',(#14291,#14292,#14293,#14294,#14295,#14296,#14297,#14298,
#14299,#14300,#14301,#14302,#14303,#14304,#14305,#14306,#14307,#14308,#14309,
#14310,#14311,#14312,#14313,#14314,#14315,#14316));
#3571=EDGE_LOOP('',(#14317,#14318,#14319,#14320,#14321));
#3572=EDGE_LOOP('',(#14322,#14323,#14324,#14325));
#3573=EDGE_LOOP('',(#14326,#14327,#14328,#14329,#14330,#14331,#14332,#14333,
#14334,#14335,#14336,#14337,#14338,#14339,#14340,#14341,#14342,#14343,#14344,
#14345,#14346,#14347,#14348,#14349,#14350,#14351));
#3574=EDGE_LOOP('',(#14352,#14353,#14354,#14355));
#3575=EDGE_LOOP('',(#14356,#14357,#14358,#14359));
#3576=EDGE_LOOP('',(#14360,#14361,#14362,#14363));
#3577=EDGE_LOOP('',(#14364,#14365,#14366,#14367));
#3578=EDGE_LOOP('',(#14368,#14369,#14370,#14371));
#3579=EDGE_LOOP('',(#14372,#14373,#14374,#14375));
#3580=EDGE_LOOP('',(#14376,#14377,#14378,#14379));
#3581=EDGE_LOOP('',(#14380,#14381,#14382,#14383));
#3582=EDGE_LOOP('',(#14384,#14385,#14386,#14387));
#3583=EDGE_LOOP('',(#14388,#14389,#14390,#14391));
#3584=EDGE_LOOP('',(#14392,#14393,#14394,#14395));
#3585=EDGE_LOOP('',(#14396,#14397,#14398,#14399));
#3586=EDGE_LOOP('',(#14400,#14401,#14402,#14403));
#3587=EDGE_LOOP('',(#14404,#14405,#14406,#14407));
#3588=EDGE_LOOP('',(#14408,#14409,#14410,#14411));
#3589=EDGE_LOOP('',(#14412,#14413,#14414,#14415));
#3590=EDGE_LOOP('',(#14416,#14417,#14418,#14419));
#3591=EDGE_LOOP('',(#14420,#14421,#14422,#14423));
#3592=EDGE_LOOP('',(#14424,#14425,#14426,#14427));
#3593=EDGE_LOOP('',(#14428,#14429,#14430,#14431));
#3594=EDGE_LOOP('',(#14432,#14433,#14434,#14435));
#3595=EDGE_LOOP('',(#14436,#14437,#14438,#14439));
#3596=EDGE_LOOP('',(#14440,#14441,#14442,#14443));
#3597=EDGE_LOOP('',(#14444,#14445,#14446,#14447));
#3598=EDGE_LOOP('',(#14448,#14449,#14450,#14451));
#3599=EDGE_LOOP('',(#14452,#14453,#14454,#14455));
#3600=EDGE_LOOP('',(#14456,#14457,#14458,#14459));
#3601=EDGE_LOOP('',(#14460,#14461,#14462,#14463));
#3602=EDGE_LOOP('',(#14464,#14465,#14466,#14467));
#3603=EDGE_LOOP('',(#14468,#14469,#14470,#14471));
#3604=EDGE_LOOP('',(#14472,#14473,#14474,#14475));
#3605=EDGE_LOOP('',(#14476,#14477,#14478,#14479));
#3606=EDGE_LOOP('',(#14480,#14481,#14482,#14483));
#3607=EDGE_LOOP('',(#14484,#14485,#14486,#14487));
#3608=EDGE_LOOP('',(#14488,#14489,#14490,#14491));
#3609=EDGE_LOOP('',(#14492,#14493,#14494,#14495));
#3610=EDGE_LOOP('',(#14496,#14497,#14498,#14499));
#3611=EDGE_LOOP('',(#14500,#14501,#14502,#14503));
#3612=EDGE_LOOP('',(#14504,#14505,#14506,#14507));
#3613=EDGE_LOOP('',(#14508,#14509,#14510,#14511));
#3614=EDGE_LOOP('',(#14512,#14513,#14514,#14515));
#3615=EDGE_LOOP('',(#14516,#14517,#14518,#14519));
#3616=EDGE_LOOP('',(#14520,#14521,#14522,#14523));
#3617=EDGE_LOOP('',(#14524,#14525,#14526,#14527));
#3618=EDGE_LOOP('',(#14528,#14529,#14530,#14531));
#3619=EDGE_LOOP('',(#14532,#14533,#14534,#14535));
#3620=EDGE_LOOP('',(#14536,#14537,#14538,#14539));
#3621=EDGE_LOOP('',(#14540,#14541,#14542,#14543));
#3622=EDGE_LOOP('',(#14544,#14545,#14546,#14547));
#3623=EDGE_LOOP('',(#14548,#14549,#14550,#14551));
#3624=EDGE_LOOP('',(#14552,#14553,#14554,#14555));
#3625=EDGE_LOOP('',(#14556,#14557,#14558,#14559));
#3626=EDGE_LOOP('',(#14560,#14561,#14562,#14563));
#3627=EDGE_LOOP('',(#14564,#14565,#14566,#14567));
#3628=EDGE_LOOP('',(#14568,#14569,#14570,#14571));
#3629=EDGE_LOOP('',(#14572,#14573,#14574,#14575));
#3630=EDGE_LOOP('',(#14576,#14577,#14578,#14579));
#3631=EDGE_LOOP('',(#14580,#14581,#14582,#14583));
#3632=EDGE_LOOP('',(#14584,#14585,#14586,#14587));
#3633=EDGE_LOOP('',(#14588,#14589,#14590,#14591));
#3634=EDGE_LOOP('',(#14592,#14593,#14594,#14595));
#3635=EDGE_LOOP('',(#14596,#14597,#14598,#14599));
#3636=EDGE_LOOP('',(#14600,#14601,#14602,#14603));
#3637=EDGE_LOOP('',(#14604,#14605,#14606,#14607));
#3638=EDGE_LOOP('',(#14608,#14609,#14610,#14611));
#3639=EDGE_LOOP('',(#14612,#14613,#14614,#14615));
#3640=EDGE_LOOP('',(#14616,#14617,#14618,#14619));
#3641=EDGE_LOOP('',(#14620,#14621,#14622,#14623));
#3642=EDGE_LOOP('',(#14624,#14625,#14626,#14627));
#3643=EDGE_LOOP('',(#14628,#14629,#14630,#14631));
#3644=EDGE_LOOP('',(#14632,#14633,#14634,#14635));
#3645=EDGE_LOOP('',(#14636,#14637,#14638,#14639));
#3646=EDGE_LOOP('',(#14640,#14641,#14642,#14643,#14644,#14645,#14646,#14647,
#14648,#14649,#14650,#14651,#14652,#14653,#14654,#14655,#14656,#14657,#14658,
#14659,#14660,#14661,#14662,#14663,#14664,#14665,#14666,#14667,#14668,#14669,
#14670,#14671,#14672,#14673,#14674,#14675,#14676,#14677,#14678,#14679,#14680,
#14681,#14682,#14683,#14684,#14685,#14686,#14687,#14688,#14689,#14690,#14691,
#14692,#14693,#14694,#14695,#14696,#14697,#14698,#14699,#14700,#14701,#14702,
#14703,#14704,#14705,#14706,#14707,#14708,#14709,#14710,#14711,#14712,#14713,
#14714));
#3647=EDGE_LOOP('',(#14715));
#3648=EDGE_LOOP('',(#14716,#14717,#14718,#14719,#14720,#14721));
#3649=EDGE_LOOP('',(#14722,#14723,#14724,#14725));
#3650=EDGE_LOOP('',(#14726));
#3651=EDGE_LOOP('',(#14727,#14728,#14729,#14730));
#3652=EDGE_LOOP('',(#14731,#14732,#14733,#14734,#14735,#14736,#14737,#14738,
#14739,#14740,#14741,#14742,#14743,#14744,#14745,#14746,#14747,#14748,#14749,
#14750,#14751,#14752,#14753,#14754,#14755,#14756,#14757,#14758,#14759,#14760,
#14761,#14762,#14763,#14764,#14765,#14766,#14767,#14768,#14769,#14770,#14771,
#14772,#14773,#14774,#14775,#14776,#14777,#14778,#14779,#14780,#14781,#14782,
#14783,#14784,#14785,#14786,#14787,#14788,#14789,#14790,#14791,#14792,#14793,
#14794,#14795,#14796,#14797,#14798,#14799,#14800,#14801,#14802,#14803,#14804,
#14805));
#3653=EDGE_LOOP('',(#14806));
#3654=LINE('',#21838,#4878);
#3655=LINE('',#21840,#4879);
#3656=LINE('',#21842,#4880);
#3657=LINE('',#21844,#4881);
#3658=LINE('',#21846,#4882);
#3659=LINE('',#21847,#4883);
#3660=LINE('',#21850,#4884);
#3661=LINE('',#21852,#4885);
#3662=LINE('',#21854,#4886);
#3663=LINE('',#21855,#4887);
#3664=LINE('',#21858,#4888);
#3665=LINE('',#21860,#4889);
#3666=LINE('',#21862,#4890);
#3667=LINE('',#21863,#4891);
#3668=LINE('',#21866,#4892);
#3669=LINE('',#21867,#4893);
#3670=LINE('',#21870,#4894);
#3671=LINE('',#21872,#4895);
#3672=LINE('',#21874,#4896);
#3673=LINE('',#21875,#4897);
#3674=LINE('',#21878,#4898);
#3675=LINE('',#21880,#4899);
#3676=LINE('',#21881,#4900);
#3677=LINE('',#21885,#4901);
#3678=LINE('',#21887,#4902);
#3679=LINE('',#21889,#4903);
#3680=LINE('',#21891,#4904);
#3681=LINE('',#21893,#4905);
#3682=LINE('',#21894,#4906);
#3683=LINE('',#21897,#4907);
#3684=LINE('',#21899,#4908);
#3685=LINE('',#21900,#4909);
#3686=LINE('',#21903,#4910);
#3687=LINE('',#21905,#4911);
#3688=LINE('',#21906,#4912);
#3689=LINE('',#21909,#4913);
#3690=LINE('',#21911,#4914);
#3691=LINE('',#21912,#4915);
#3692=LINE('',#21916,#4916);
#3693=LINE('',#21918,#4917);
#3694=LINE('',#21920,#4918);
#3695=LINE('',#21922,#4919);
#3696=LINE('',#21924,#4920);
#3697=LINE('',#21925,#4921);
#3698=LINE('',#21928,#4922);
#3699=LINE('',#21930,#4923);
#3700=LINE('',#21932,#4924);
#3701=LINE('',#21933,#4925);
#3702=LINE('',#21936,#4926);
#3703=LINE('',#21937,#4927);
#3704=LINE('',#21940,#4928);
#3705=LINE('',#21942,#4929);
#3706=LINE('',#21943,#4930);
#3707=LINE('',#21947,#4931);
#3708=LINE('',#21949,#4932);
#3709=LINE('',#21951,#4933);
#3710=LINE('',#21953,#4934);
#3711=LINE('',#21955,#4935);
#3712=LINE('',#21956,#4936);
#3713=LINE('',#21959,#4937);
#3714=LINE('',#21961,#4938);
#3715=LINE('',#21963,#4939);
#3716=LINE('',#21965,#4940);
#3717=LINE('',#21966,#4941);
#3718=LINE('',#21969,#4942);
#3719=LINE('',#21970,#4943);
#3720=LINE('',#21973,#4944);
#3721=LINE('',#21975,#4945);
#3722=LINE('',#21977,#4946);
#3723=LINE('',#21978,#4947);
#3724=LINE('',#21981,#4948);
#3725=LINE('',#21983,#4949);
#3726=LINE('',#21984,#4950);
#3727=LINE('',#21989,#4951);
#3728=LINE('',#21993,#4952);
#3729=LINE('',#22000,#4953);
#3730=LINE('',#22004,#4954);
#3731=LINE('',#22118,#4955);
#3732=LINE('',#22148,#4956);
#3733=LINE('',#22175,#4957);
#3734=LINE('',#22177,#4958);
#3735=LINE('',#22179,#4959);
#3736=LINE('',#22181,#4960);
#3737=LINE('',#22183,#4961);
#3738=LINE('',#22184,#4962);
#3739=LINE('',#22187,#4963);
#3740=LINE('',#22189,#4964);
#3741=LINE('',#22190,#4965);
#3742=LINE('',#22193,#4966);
#3743=LINE('',#22195,#4967);
#3744=LINE('',#22197,#4968);
#3745=LINE('',#22198,#4969);
#3746=LINE('',#22201,#4970);
#3747=LINE('',#22203,#4971);
#3748=LINE('',#22204,#4972);
#3749=LINE('',#22208,#4973);
#3750=LINE('',#22210,#4974);
#3751=LINE('',#22212,#4975);
#3752=LINE('',#22214,#4976);
#3753=LINE('',#22216,#4977);
#3754=LINE('',#22217,#4978);
#3755=LINE('',#22220,#4979);
#3756=LINE('',#22222,#4980);
#3757=LINE('',#22224,#4981);
#3758=LINE('',#22225,#4982);
#3759=LINE('',#22228,#4983);
#3760=LINE('',#22229,#4984);
#3761=LINE('',#22232,#4985);
#3762=LINE('',#22234,#4986);
#3763=LINE('',#22235,#4987);
#3764=LINE('',#22239,#4988);
#3765=LINE('',#22245,#4989);
#3766=LINE('',#22246,#4990);
#3767=LINE('',#22247,#4991);
#3768=LINE('',#22253,#4992);
#3769=LINE('',#22255,#4993);
#3770=LINE('',#22257,#4994);
#3771=LINE('',#22258,#4995);
#3772=LINE('',#22261,#4996);
#3773=LINE('',#22262,#4997);
#3774=LINE('',#22265,#4998);
#3775=LINE('',#22269,#4999);
#3776=LINE('',#22270,#5000);
#3777=LINE('',#22273,#5001);
#3778=LINE('',#22276,#5002);
#3779=LINE('',#22279,#5003);
#3780=LINE('',#22281,#5004);
#3781=LINE('',#22283,#5005);
#3782=LINE('',#22284,#5006);
#3783=LINE('',#22288,#5007);
#3784=LINE('',#22294,#5008);
#3785=LINE('',#22295,#5009);
#3786=LINE('',#22296,#5010);
#3787=LINE('',#22300,#5011);
#3788=LINE('',#22305,#5012);
#3789=LINE('',#22306,#5013);
#3790=LINE('',#22307,#5014);
#3791=LINE('',#22309,#5015);
#3792=LINE('',#22311,#5016);
#3793=LINE('',#22313,#5017);
#3794=LINE('',#22315,#5018);
#3795=LINE('',#22319,#5019);
#3796=LINE('',#22320,#5020);
#3797=LINE('',#22323,#5021);
#3798=LINE('',#22328,#5022);
#3799=LINE('',#22329,#5023);
#3800=LINE('',#22332,#5024);
#3801=LINE('',#22333,#5025);
#3802=LINE('',#22336,#5026);
#3803=LINE('',#22337,#5027);
#3804=LINE('',#22340,#5028);
#3805=LINE('',#22345,#5029);
#3806=LINE('',#22346,#5030);
#3807=LINE('',#22349,#5031);
#3808=LINE('',#22350,#5032);
#3809=LINE('',#22354,#5033);
#3810=LINE('',#22360,#5034);
#3811=LINE('',#22361,#5035);
#3812=LINE('',#22362,#5036);
#3813=LINE('',#22365,#5037);
#3814=LINE('',#22370,#5038);
#3815=LINE('',#22371,#5039);
#3816=LINE('',#22374,#5040);
#3817=LINE('',#22376,#5041);
#3818=LINE('',#22377,#5042);
#3819=LINE('',#22381,#5043);
#3820=LINE('',#22385,#5044);
#3821=LINE('',#22387,#5045);
#3822=LINE('',#22388,#5046);
#3823=LINE('',#22391,#5047);
#3824=LINE('',#22392,#5048);
#3825=LINE('',#22395,#5049);
#3826=LINE('',#22397,#5050);
#3827=LINE('',#22398,#5051);
#3828=LINE('',#22401,#5052);
#3829=LINE('',#22405,#5053);
#3830=LINE('',#22482,#5054);
#3831=LINE('',#22505,#5055);
#3832=LINE('',#22512,#5056);
#3833=LINE('',#22514,#5057);
#3834=LINE('',#22520,#5058);
#3835=LINE('',#22522,#5059);
#3836=LINE('',#22523,#5060);
#3837=LINE('',#22526,#5061);
#3838=LINE('',#22528,#5062);
#3839=LINE('',#22529,#5063);
#3840=LINE('',#22533,#5064);
#3841=LINE('',#22539,#5065);
#3842=LINE('',#22540,#5066);
#3843=LINE('',#22541,#5067);
#3844=LINE('',#22544,#5068);
#3845=LINE('',#22549,#5069);
#3846=LINE('',#22550,#5070);
#3847=LINE('',#22553,#5071);
#3848=LINE('',#22555,#5072);
#3849=LINE('',#22556,#5073);
#3850=LINE('',#22560,#5074);
#3851=LINE('',#22564,#5075);
#3852=LINE('',#22565,#5076);
#3853=LINE('',#22568,#5077);
#3854=LINE('',#22570,#5078);
#3855=LINE('',#22571,#5079);
#3856=LINE('',#22575,#5080);
#3857=LINE('',#22579,#5081);
#3858=LINE('',#22580,#5082);
#3859=LINE('',#22583,#5083);
#3860=LINE('',#22585,#5084);
#3861=LINE('',#22586,#5085);
#3862=LINE('',#22589,#5086);
#3863=LINE('',#22593,#5087);
#3864=LINE('',#22596,#5088);
#3865=LINE('',#22597,#5089);
#3866=LINE('',#22601,#5090);
#3867=LINE('',#22605,#5091);
#3868=LINE('',#22606,#5092);
#3869=LINE('',#22609,#5093);
#3870=LINE('',#22613,#5094);
#3871=LINE('',#22614,#5095);
#3872=LINE('',#22619,#5096);
#3873=LINE('',#22622,#5097);
#3874=LINE('',#22625,#5098);
#3875=LINE('',#22626,#5099);
#3876=LINE('',#22629,#5100);
#3877=LINE('',#22632,#5101);
#3878=LINE('',#22637,#5102);
#3879=LINE('',#22640,#5103);
#3880=LINE('',#22641,#5104);
#3881=LINE('',#22645,#5105);
#3882=LINE('',#22647,#5106);
#3883=LINE('',#22652,#5107);
#3884=LINE('',#22657,#5108);
#3885=LINE('',#22659,#5109);
#3886=LINE('',#22662,#5110);
#3887=LINE('',#22665,#5111);
#3888=LINE('',#22667,#5112);
#3889=LINE('',#22678,#5113);
#3890=LINE('',#22705,#5114);
#3891=LINE('',#22733,#5115);
#3892=LINE('',#22777,#5116);
#3893=LINE('',#22779,#5117);
#3894=LINE('',#22781,#5118);
#3895=LINE('',#22784,#5119);
#3896=LINE('',#22828,#5120);
#3897=LINE('',#22832,#5121);
#3898=LINE('',#22875,#5122);
#3899=LINE('',#22882,#5123);
#3900=LINE('',#22886,#5124);
#3901=LINE('',#22893,#5125);
#3902=LINE('',#22897,#5126);
#3903=LINE('',#22898,#5127);
#3904=LINE('',#22902,#5128);
#3905=LINE('',#22908,#5129);
#3906=LINE('',#22911,#5130);
#3907=LINE('',#22913,#5131);
#3908=LINE('',#22921,#5132);
#3909=LINE('',#22927,#5133);
#3910=LINE('',#22934,#5134);
#3911=LINE('',#22940,#5135);
#3912=LINE('',#22946,#5136);
#3913=LINE('',#22952,#5137);
#3914=LINE('',#22958,#5138);
#3915=LINE('',#22965,#5139);
#3916=LINE('',#22967,#5140);
#3917=LINE('',#22969,#5141);
#3918=LINE('',#22971,#5142);
#3919=LINE('',#22973,#5143);
#3920=LINE('',#22974,#5144);
#3921=LINE('',#22977,#5145);
#3922=LINE('',#22979,#5146);
#3923=LINE('',#22981,#5147);
#3924=LINE('',#22983,#5148);
#3925=LINE('',#22984,#5149);
#3926=LINE('',#22987,#5150);
#3927=LINE('',#22989,#5151);
#3928=LINE('',#22991,#5152);
#3929=LINE('',#22993,#5153);
#3930=LINE('',#22995,#5154);
#3931=LINE('',#22997,#5155);
#3932=LINE('',#22998,#5156);
#3933=LINE('',#23001,#5157);
#3934=LINE('',#23002,#5158);
#3935=LINE('',#23005,#5159);
#3936=LINE('',#23007,#5160);
#3937=LINE('',#23009,#5161);
#3938=LINE('',#23011,#5162);
#3939=LINE('',#23012,#5163);
#3940=LINE('',#23014,#5164);
#3941=LINE('',#23017,#5165);
#3942=LINE('',#23019,#5166);
#3943=LINE('',#23021,#5167);
#3944=LINE('',#23023,#5168);
#3945=LINE('',#23025,#5169);
#3946=LINE('',#23026,#5170);
#3947=LINE('',#23029,#5171);
#3948=LINE('',#23031,#5172);
#3949=LINE('',#23032,#5173);
#3950=LINE('',#23035,#5174);
#3951=LINE('',#23037,#5175);
#3952=LINE('',#23039,#5176);
#3953=LINE('',#23041,#5177);
#3954=LINE('',#23043,#5178);
#3955=LINE('',#23044,#5179);
#3956=LINE('',#23048,#5180);
#3957=LINE('',#23049,#5181);
#3958=LINE('',#23051,#5182);
#3959=LINE('',#23053,#5183);
#3960=LINE('',#23054,#5184);
#3961=LINE('',#23057,#5185);
#3962=LINE('',#23059,#5186);
#3963=LINE('',#23061,#5187);
#3964=LINE('',#23063,#5188);
#3965=LINE('',#23064,#5189);
#3966=LINE('',#23067,#5190);
#3967=LINE('',#23068,#5191);
#3968=LINE('',#23071,#5192);
#3969=LINE('',#23073,#5193);
#3970=LINE('',#23074,#5194);
#3971=LINE('',#23077,#5195);
#3972=LINE('',#23078,#5196);
#3973=LINE('',#23081,#5197);
#3974=LINE('',#23083,#5198);
#3975=LINE('',#23085,#5199);
#3976=LINE('',#23087,#5200);
#3977=LINE('',#23089,#5201);
#3978=LINE('',#23090,#5202);
#3979=LINE('',#23094,#5203);
#3980=LINE('',#23095,#5204);
#3981=LINE('',#23097,#5205);
#3982=LINE('',#23099,#5206);
#3983=LINE('',#23100,#5207);
#3984=LINE('',#23103,#5208);
#3985=LINE('',#23105,#5209);
#3986=LINE('',#23107,#5210);
#3987=LINE('',#23109,#5211);
#3988=LINE('',#23110,#5212);
#3989=LINE('',#23113,#5213);
#3990=LINE('',#23114,#5214);
#3991=LINE('',#23117,#5215);
#3992=LINE('',#23119,#5216);
#3993=LINE('',#23120,#5217);
#3994=LINE('',#23123,#5218);
#3995=LINE('',#23125,#5219);
#3996=LINE('',#23126,#5220);
#3997=LINE('',#23129,#5221);
#3998=LINE('',#23131,#5222);
#3999=LINE('',#23133,#5223);
#4000=LINE('',#23134,#5224);
#4001=LINE('',#23135,#5225);
#4002=LINE('',#23138,#5226);
#4003=LINE('',#23140,#5227);
#4004=LINE('',#23142,#5228);
#4005=LINE('',#23144,#5229);
#4006=LINE('',#23146,#5230);
#4007=LINE('',#23148,#5231);
#4008=LINE('',#23149,#5232);
#4009=LINE('',#23152,#5233);
#4010=LINE('',#23153,#5234);
#4011=LINE('',#23156,#5235);
#4012=LINE('',#23158,#5236);
#4013=LINE('',#23160,#5237);
#4014=LINE('',#23162,#5238);
#4015=LINE('',#23163,#5239);
#4016=LINE('',#23165,#5240);
#4017=LINE('',#23167,#5241);
#4018=LINE('',#23169,#5242);
#4019=LINE('',#23170,#5243);
#4020=LINE('',#23173,#5244);
#4021=LINE('',#23174,#5245);
#4022=LINE('',#23176,#5246);
#4023=LINE('',#23179,#5247);
#4024=LINE('',#23180,#5248);
#4025=LINE('',#23181,#5249);
#4026=LINE('',#23183,#5250);
#4027=LINE('',#23184,#5251);
#4028=LINE('',#23187,#5252);
#4029=LINE('',#23189,#5253);
#4030=LINE('',#23191,#5254);
#4031=LINE('',#23192,#5255);
#4032=LINE('',#23195,#5256);
#4033=LINE('',#23196,#5257);
#4034=LINE('',#23200,#5258);
#4035=LINE('',#23201,#5259);
#4036=LINE('',#23203,#5260);
#4037=LINE('',#23218,#5261);
#4038=LINE('',#23221,#5262);
#4039=LINE('',#23222,#5263);
#4040=LINE('',#23225,#5264);
#4041=LINE('',#23226,#5265);
#4042=LINE('',#23229,#5266);
#4043=LINE('',#23230,#5267);
#4044=LINE('',#23231,#5268);
#4045=LINE('',#23238,#5269);
#4046=LINE('',#23247,#5270);
#4047=LINE('',#23250,#5271);
#4048=LINE('',#23255,#5272);
#4049=LINE('',#23263,#5273);
#4050=LINE('',#23271,#5274);
#4051=LINE('',#23274,#5275);
#4052=LINE('',#23277,#5276);
#4053=LINE('',#23280,#5277);
#4054=LINE('',#23287,#5278);
#4055=LINE('',#23291,#5279);
#4056=LINE('',#23297,#5280);
#4057=LINE('',#23304,#5281);
#4058=LINE('',#23308,#5282);
#4059=LINE('',#23314,#5283);
#4060=LINE('',#23319,#5284);
#4061=LINE('',#23322,#5285);
#4062=LINE('',#23327,#5286);
#4063=LINE('',#23330,#5287);
#4064=LINE('',#23335,#5288);
#4065=LINE('',#23340,#5289);
#4066=LINE('',#23345,#5290);
#4067=LINE('',#23347,#5291);
#4068=LINE('',#23349,#5292);
#4069=LINE('',#23350,#5293);
#4070=LINE('',#23362,#5294);
#4071=LINE('',#23365,#5295);
#4072=LINE('',#23368,#5296);
#4073=LINE('',#23370,#5297);
#4074=LINE('',#23372,#5298);
#4075=LINE('',#23373,#5299);
#4076=LINE('',#23375,#5300);
#4077=LINE('',#23377,#5301);
#4078=LINE('',#23380,#5302);
#4079=LINE('',#23382,#5303);
#4080=LINE('',#23384,#5304);
#4081=LINE('',#23395,#5305);
#4082=LINE('',#23399,#5306);
#4083=LINE('',#23403,#5307);
#4084=LINE('',#23409,#5308);
#4085=LINE('',#23455,#5309);
#4086=LINE('',#23502,#5310);
#4087=LINE('',#23592,#5311);
#4088=LINE('',#23624,#5312);
#4089=LINE('',#23993,#5313);
#4090=LINE('',#24041,#5314);
#4091=LINE('',#24045,#5315);
#4092=LINE('',#24085,#5316);
#4093=LINE('',#24449,#5317);
#4094=LINE('',#24451,#5318);
#4095=LINE('',#24454,#5319);
#4096=LINE('',#24499,#5320);
#4097=LINE('',#24505,#5321);
#4098=LINE('',#24506,#5322);
#4099=LINE('',#24509,#5323);
#4100=LINE('',#24511,#5324);
#4101=LINE('',#24517,#5325);
#4102=LINE('',#24524,#5326);
#4103=LINE('',#24528,#5327);
#4104=LINE('',#24538,#5328);
#4105=LINE('',#24543,#5329);
#4106=LINE('',#24547,#5330);
#4107=LINE('',#24550,#5331);
#4108=LINE('',#24556,#5332);
#4109=LINE('',#24563,#5333);
#4110=LINE('',#24579,#5334);
#4111=LINE('',#24585,#5335);
#4112=LINE('',#24609,#5336);
#4113=LINE('',#24657,#5337);
#4114=LINE('',#24705,#5338);
#4115=LINE('',#24759,#5339);
#4116=LINE('',#24807,#5340);
#4117=LINE('',#24855,#5341);
#4118=LINE('',#24874,#5342);
#4119=LINE('',#24899,#5343);
#4120=LINE('',#24923,#5344);
#4121=LINE('',#24948,#5345);
#4122=LINE('',#24973,#5346);
#4123=LINE('',#25635,#5347);
#4124=LINE('',#25639,#5348);
#4125=LINE('',#25643,#5349);
#4126=LINE('',#25647,#5350);
#4127=LINE('',#25651,#5351);
#4128=LINE('',#25654,#5352);
#4129=LINE('',#25659,#5353);
#4130=LINE('',#25717,#5354);
#4131=LINE('',#25719,#5355);
#4132=LINE('',#25720,#5356);
#4133=LINE('',#25723,#5357);
#4134=LINE('',#25724,#5358);
#4135=LINE('',#25727,#5359);
#4136=LINE('',#25728,#5360);
#4137=LINE('',#25731,#5361);
#4138=LINE('',#25732,#5362);
#4139=LINE('',#25735,#5363);
#4140=LINE('',#25736,#5364);
#4141=LINE('',#25739,#5365);
#4142=LINE('',#25740,#5366);
#4143=LINE('',#25743,#5367);
#4144=LINE('',#25744,#5368);
#4145=LINE('',#25747,#5369);
#4146=LINE('',#25748,#5370);
#4147=LINE('',#25751,#5371);
#4148=LINE('',#25752,#5372);
#4149=LINE('',#25754,#5373);
#4150=LINE('',#25756,#5374);
#4151=LINE('',#25759,#5375);
#4152=LINE('',#25762,#5376);
#4153=LINE('',#25763,#5377);
#4154=LINE('',#25765,#5378);
#4155=LINE('',#25767,#5379);
#4156=LINE('',#25770,#5380);
#4157=LINE('',#25771,#5381);
#4158=LINE('',#25773,#5382);
#4159=LINE('',#25777,#5383);
#4160=LINE('',#25785,#5384);
#4161=LINE('',#25791,#5385);
#4162=LINE('',#25797,#5386);
#4163=LINE('',#25821,#5387);
#4164=LINE('',#25869,#5388);
#4165=LINE('',#25917,#5389);
#4166=LINE('',#25971,#5390);
#4167=LINE('',#26019,#5391);
#4168=LINE('',#26029,#5392);
#4169=LINE('',#26054,#5393);
#4170=LINE('',#26079,#5394);
#4171=LINE('',#26104,#5395);
#4172=LINE('',#26676,#5396);
#4173=LINE('',#26680,#5397);
#4174=LINE('',#26684,#5398);
#4175=LINE('',#26688,#5399);
#4176=LINE('',#26692,#5400);
#4177=LINE('',#26695,#5401);
#4178=LINE('',#26700,#5402);
#4179=LINE('',#26758,#5403);
#4180=LINE('',#26760,#5404);
#4181=LINE('',#26761,#5405);
#4182=LINE('',#26764,#5406);
#4183=LINE('',#26765,#5407);
#4184=LINE('',#26768,#5408);
#4185=LINE('',#26769,#5409);
#4186=LINE('',#26772,#5410);
#4187=LINE('',#26773,#5411);
#4188=LINE('',#26776,#5412);
#4189=LINE('',#26777,#5413);
#4190=LINE('',#26780,#5414);
#4191=LINE('',#26781,#5415);
#4192=LINE('',#26784,#5416);
#4193=LINE('',#26785,#5417);
#4194=LINE('',#26788,#5418);
#4195=LINE('',#26789,#5419);
#4196=LINE('',#26792,#5420);
#4197=LINE('',#26793,#5421);
#4198=LINE('',#26795,#5422);
#4199=LINE('',#26797,#5423);
#4200=LINE('',#26800,#5424);
#4201=LINE('',#26803,#5425);
#4202=LINE('',#26804,#5426);
#4203=LINE('',#26806,#5427);
#4204=LINE('',#26808,#5428);
#4205=LINE('',#26811,#5429);
#4206=LINE('',#26812,#5430);
#4207=LINE('',#26814,#5431);
#4208=LINE('',#26818,#5432);
#4209=LINE('',#26826,#5433);
#4210=LINE('',#26832,#5434);
#4211=LINE('',#26838,#5435);
#4212=LINE('',#26840,#5436);
#4213=LINE('',#26842,#5437);
#4214=LINE('',#26844,#5438);
#4215=LINE('',#26846,#5439);
#4216=LINE('',#26847,#5440);
#4217=LINE('',#26850,#5441);
#4218=LINE('',#26852,#5442);
#4219=LINE('',#26854,#5443);
#4220=LINE('',#26855,#5444);
#4221=LINE('',#26858,#5445);
#4222=LINE('',#26860,#5446);
#4223=LINE('',#26861,#5447);
#4224=LINE('',#26864,#5448);
#4225=LINE('',#26866,#5449);
#4226=LINE('',#26867,#5450);
#4227=LINE('',#26871,#5451);
#4228=LINE('',#26873,#5452);
#4229=LINE('',#26875,#5453);
#4230=LINE('',#26876,#5454);
#4231=LINE('',#26879,#5455);
#4232=LINE('',#26881,#5456);
#4233=LINE('',#26882,#5457);
#4234=LINE('',#26885,#5458);
#4235=LINE('',#26887,#5459);
#4236=LINE('',#26888,#5460);
#4237=LINE('',#26891,#5461);
#4238=LINE('',#26896,#5462);
#4239=LINE('',#27019,#5463);
#4240=LINE('',#27088,#5464);
#4241=LINE('',#27127,#5465);
#4242=LINE('',#27141,#5466);
#4243=LINE('',#27145,#5467);
#4244=LINE('',#27251,#5468);
#4245=LINE('',#27292,#5469);
#4246=LINE('',#27296,#5470);
#4247=LINE('',#27304,#5471);
#4248=LINE('',#27306,#5472);
#4249=LINE('',#27308,#5473);
#4250=LINE('',#27309,#5474);
#4251=LINE('',#27313,#5475);
#4252=LINE('',#27314,#5476);
#4253=LINE('',#27315,#5477);
#4254=LINE('',#27317,#5478);
#4255=LINE('',#27318,#5479);
#4256=LINE('',#27320,#5480);
#4257=LINE('',#27321,#5481);
#4258=LINE('',#27324,#5482);
#4259=LINE('',#27326,#5483);
#4260=LINE('',#27327,#5484);
#4261=LINE('',#27332,#5485);
#4262=LINE('',#27334,#5486);
#4263=LINE('',#27336,#5487);
#4264=LINE('',#27338,#5488);
#4265=LINE('',#27340,#5489);
#4266=LINE('',#27341,#5490);
#4267=LINE('',#27344,#5491);
#4268=LINE('',#27346,#5492);
#4269=LINE('',#27348,#5493);
#4270=LINE('',#27350,#5494);
#4271=LINE('',#27351,#5495);
#4272=LINE('',#27354,#5496);
#4273=LINE('',#27356,#5497);
#4274=LINE('',#27358,#5498);
#4275=LINE('',#27359,#5499);
#4276=LINE('',#27362,#5500);
#4277=LINE('',#27363,#5501);
#4278=LINE('',#27366,#5502);
#4279=LINE('',#27368,#5503);
#4280=LINE('',#27369,#5504);
#4281=LINE('',#27371,#5505);
#4282=LINE('',#27373,#5506);
#4283=LINE('',#27375,#5507);
#4284=LINE('',#27377,#5508);
#4285=LINE('',#27378,#5509);
#4286=LINE('',#27380,#5510);
#4287=LINE('',#27382,#5511);
#4288=LINE('',#27383,#5512);
#4289=LINE('',#27385,#5513);
#4290=LINE('',#27389,#5514);
#4291=LINE('',#27391,#5515);
#4292=LINE('',#27392,#5516);
#4293=LINE('',#27393,#5517);
#4294=LINE('',#27396,#5518);
#4295=LINE('',#27397,#5519);
#4296=LINE('',#27400,#5520);
#4297=LINE('',#27402,#5521);
#4298=LINE('',#27404,#5522);
#4299=LINE('',#27406,#5523);
#4300=LINE('',#27408,#5524);
#4301=LINE('',#27409,#5525);
#4302=LINE('',#27412,#5526);
#4303=LINE('',#27416,#5527);
#4304=LINE('',#27417,#5528);
#4305=LINE('',#27420,#5529);
#4306=LINE('',#27421,#5530);
#4307=LINE('',#27423,#5531);
#4308=LINE('',#27424,#5532);
#4309=LINE('',#27427,#5533);
#4310=LINE('',#27429,#5534);
#4311=LINE('',#27430,#5535);
#4312=LINE('',#27434,#5536);
#4313=LINE('',#27436,#5537);
#4314=LINE('',#27438,#5538);
#4315=LINE('',#27439,#5539);
#4316=LINE('',#27443,#5540);
#4317=LINE('',#27445,#5541);
#4318=LINE('',#27447,#5542);
#4319=LINE('',#27448,#5543);
#4320=LINE('',#27452,#5544);
#4321=LINE('',#27453,#5545);
#4322=LINE('',#27454,#5546);
#4323=LINE('',#27455,#5547);
#4324=LINE('',#27457,#5548);
#4325=LINE('',#27459,#5549);
#4326=LINE('',#27461,#5550);
#4327=LINE('',#27462,#5551);
#4328=LINE('',#27465,#5552);
#4329=LINE('',#27466,#5553);
#4330=LINE('',#27469,#5554);
#4331=LINE('',#27470,#5555);
#4332=LINE('',#27472,#5556);
#4333=LINE('',#27473,#5557);
#4334=LINE('',#27484,#5558);
#4335=LINE('',#27488,#5559);
#4336=LINE('',#27491,#5560);
#4337=LINE('',#27495,#5561);
#4338=LINE('',#27499,#5562);
#4339=LINE('',#27503,#5563);
#4340=LINE('',#27515,#5564);
#4341=LINE('',#27518,#5565);
#4342=LINE('',#27523,#5566);
#4343=LINE('',#27527,#5567);
#4344=LINE('',#27529,#5568);
#4345=LINE('',#27531,#5569);
#4346=LINE('',#27532,#5570);
#4347=LINE('',#27538,#5571);
#4348=LINE('',#27540,#5572);
#4349=LINE('',#27541,#5573);
#4350=LINE('',#27542,#5574);
#4351=LINE('',#27544,#5575);
#4352=LINE('',#27545,#5576);
#4353=LINE('',#27546,#5577);
#4354=LINE('',#27550,#5578);
#4355=LINE('',#27551,#5579);
#4356=LINE('',#27554,#5580);
#4357=LINE('',#27559,#5581);
#4358=LINE('',#27563,#5582);
#4359=LINE('',#27566,#5583);
#4360=LINE('',#27569,#5584);
#4361=LINE('',#27571,#5585);
#4362=LINE('',#27574,#5586);
#4363=LINE('',#27578,#5587);
#4364=LINE('',#27582,#5588);
#4365=LINE('',#27588,#5589);
#4366=LINE('',#27612,#5590);
#4367=LINE('',#27660,#5591);
#4368=LINE('',#27708,#5592);
#4369=LINE('',#27762,#5593);
#4370=LINE('',#27810,#5594);
#4371=LINE('',#27858,#5595);
#4372=LINE('',#27906,#5596);
#4373=LINE('',#27957,#5597);
#4374=LINE('',#28005,#5598);
#4375=LINE('',#28053,#5599);
#4376=LINE('',#28107,#5600);
#4377=LINE('',#28155,#5601);
#4378=LINE('',#28203,#5602);
#4379=LINE('',#28257,#5603);
#4380=LINE('',#28305,#5604);
#4381=LINE('',#28353,#5605);
#4382=LINE('',#28407,#5606);
#4383=LINE('',#28455,#5607);
#4384=LINE('',#28503,#5608);
#4385=LINE('',#28557,#5609);
#4386=LINE('',#28605,#5610);
#4387=LINE('',#28653,#5611);
#4388=LINE('',#28704,#5612);
#4389=LINE('',#28754,#5613);
#4390=LINE('',#28775,#5614);
#4391=LINE('',#28799,#5615);
#4392=LINE('',#28824,#5616);
#4393=LINE('',#28848,#5617);
#4394=LINE('',#28873,#5618);
#4395=LINE('',#28898,#5619);
#4396=LINE('',#28922,#5620);
#4397=LINE('',#28947,#5621);
#4398=LINE('',#28972,#5622);
#4399=LINE('',#28996,#5623);
#4400=LINE('',#29021,#5624);
#4401=LINE('',#29046,#5625);
#4402=LINE('',#29070,#5626);
#4403=LINE('',#29095,#5627);
#4404=LINE('',#29120,#5628);
#4405=LINE('',#29144,#5629);
#4406=LINE('',#29169,#5630);
#4407=LINE('',#29193,#5631);
#4408=LINE('',#29218,#5632);
#4409=LINE('',#29242,#5633);
#4410=LINE('',#29267,#5634);
#4411=LINE('',#29292,#5635);
#4412=LINE('',#29316,#5636);
#4413=LINE('',#29318,#5637);
#4414=LINE('',#29320,#5638);
#4415=LINE('',#29321,#5639);
#4416=LINE('',#29324,#5640);
#4417=LINE('',#29326,#5641);
#4418=LINE('',#29327,#5642);
#4419=LINE('',#29330,#5643);
#4420=LINE('',#29332,#5644);
#4421=LINE('',#29333,#5645);
#4422=LINE('',#29335,#5646);
#4423=LINE('',#29336,#5647);
#4424=LINE('',#29342,#5648);
#4425=LINE('',#30818,#5649);
#4426=LINE('',#30823,#5650);
#4427=LINE('',#30830,#5651);
#4428=LINE('',#30841,#5652);
#4429=LINE('',#30846,#5653);
#4430=LINE('',#30853,#5654);
#4431=LINE('',#30864,#5655);
#4432=LINE('',#30869,#5656);
#4433=LINE('',#30876,#5657);
#4434=LINE('',#30887,#5658);
#4435=LINE('',#30892,#5659);
#4436=LINE('',#30899,#5660);
#4437=LINE('',#30910,#5661);
#4438=LINE('',#30915,#5662);
#4439=LINE('',#30922,#5663);
#4440=LINE('',#30933,#5664);
#4441=LINE('',#30938,#5665);
#4442=LINE('',#30945,#5666);
#4443=LINE('',#30956,#5667);
#4444=LINE('',#30961,#5668);
#4445=LINE('',#30968,#5669);
#4446=LINE('',#30979,#5670);
#4447=LINE('',#30984,#5671);
#4448=LINE('',#30991,#5672);
#4449=LINE('',#31002,#5673);
#4450=LINE('',#31007,#5674);
#4451=LINE('',#31014,#5675);
#4452=LINE('',#31025,#5676);
#4453=LINE('',#31030,#5677);
#4454=LINE('',#31037,#5678);
#4455=LINE('',#31048,#5679);
#4456=LINE('',#31053,#5680);
#4457=LINE('',#31060,#5681);
#4458=LINE('',#31071,#5682);
#4459=LINE('',#31076,#5683);
#4460=LINE('',#31083,#5684);
#4461=LINE('',#31094,#5685);
#4462=LINE('',#31099,#5686);
#4463=LINE('',#31106,#5687);
#4464=LINE('',#31117,#5688);
#4465=LINE('',#31122,#5689);
#4466=LINE('',#31129,#5690);
#4467=LINE('',#31140,#5691);
#4468=LINE('',#31145,#5692);
#4469=LINE('',#31152,#5693);
#4470=LINE('',#31163,#5694);
#4471=LINE('',#31168,#5695);
#4472=LINE('',#31175,#5696);
#4473=LINE('',#31186,#5697);
#4474=LINE('',#31191,#5698);
#4475=LINE('',#31198,#5699);
#4476=LINE('',#31209,#5700);
#4477=LINE('',#31214,#5701);
#4478=LINE('',#31221,#5702);
#4479=LINE('',#31232,#5703);
#4480=LINE('',#31237,#5704);
#4481=LINE('',#31244,#5705);
#4482=LINE('',#31255,#5706);
#4483=LINE('',#31260,#5707);
#4484=LINE('',#31267,#5708);
#4485=LINE('',#31278,#5709);
#4486=LINE('',#31283,#5710);
#4487=LINE('',#31290,#5711);
#4488=LINE('',#31301,#5712);
#4489=LINE('',#31306,#5713);
#4490=LINE('',#31313,#5714);
#4491=LINE('',#31324,#5715);
#4492=LINE('',#31329,#5716);
#4493=LINE('',#31336,#5717);
#4494=LINE('',#31347,#5718);
#4495=LINE('',#31352,#5719);
#4496=LINE('',#31359,#5720);
#4497=LINE('',#31370,#5721);
#4498=LINE('',#31375,#5722);
#4499=LINE('',#31382,#5723);
#4500=LINE('',#31393,#5724);
#4501=LINE('',#31398,#5725);
#4502=LINE('',#31405,#5726);
#4503=LINE('',#31416,#5727);
#4504=LINE('',#31421,#5728);
#4505=LINE('',#31428,#5729);
#4506=LINE('',#31439,#5730);
#4507=LINE('',#31444,#5731);
#4508=LINE('',#31451,#5732);
#4509=LINE('',#31462,#5733);
#4510=LINE('',#31467,#5734);
#4511=LINE('',#31474,#5735);
#4512=LINE('',#31485,#5736);
#4513=LINE('',#31490,#5737);
#4514=LINE('',#31497,#5738);
#4515=LINE('',#31593,#5739);
#4516=LINE('',#31599,#5740);
#4517=LINE('',#31606,#5741);
#4518=LINE('',#32272,#5742);
#4519=LINE('',#32296,#5743);
#4520=LINE('',#32344,#5744);
#4521=LINE('',#32392,#5745);
#4522=LINE('',#32443,#5746);
#4523=LINE('',#32494,#5747);
#4524=LINE('',#32542,#5748);
#4525=LINE('',#32590,#5749);
#4526=LINE('',#32644,#5750);
#4527=LINE('',#32692,#5751);
#4528=LINE('',#32740,#5752);
#4529=LINE('',#32794,#5753);
#4530=LINE('',#32842,#5754);
#4531=LINE('',#32890,#5755);
#4532=LINE('',#32938,#5756);
#4533=LINE('',#32992,#5757);
#4534=LINE('',#33040,#5758);
#4535=LINE('',#33088,#5759);
#4536=LINE('',#33142,#5760);
#4537=LINE('',#33190,#5761);
#4538=LINE('',#33238,#5762);
#4539=LINE('',#33292,#5763);
#4540=LINE('',#33340,#5764);
#4541=LINE('',#33358,#5765);
#4542=LINE('',#33382,#5766);
#4543=LINE('',#33407,#5767);
#4544=LINE('',#33432,#5768);
#4545=LINE('',#33456,#5769);
#4546=LINE('',#33481,#5770);
#4547=LINE('',#33506,#5771);
#4548=LINE('',#33530,#5772);
#4549=LINE('',#33555,#5773);
#4550=LINE('',#33580,#5774);
#4551=LINE('',#33604,#5775);
#4552=LINE('',#33628,#5776);
#4553=LINE('',#33653,#5777);
#4554=LINE('',#33678,#5778);
#4555=LINE('',#33702,#5779);
#4556=LINE('',#33727,#5780);
#4557=LINE('',#33752,#5781);
#4558=LINE('',#33776,#5782);
#4559=LINE('',#33801,#5783);
#4560=LINE('',#33825,#5784);
#4561=LINE('',#33850,#5785);
#4562=LINE('',#35306,#5786);
#4563=LINE('',#35308,#5787);
#4564=LINE('',#35312,#5788);
#4565=LINE('',#35314,#5789);
#4566=LINE('',#35318,#5790);
#4567=LINE('',#35320,#5791);
#4568=LINE('',#35324,#5792);
#4569=LINE('',#35326,#5793);
#4570=LINE('',#35330,#5794);
#4571=LINE('',#35332,#5795);
#4572=LINE('',#35336,#5796);
#4573=LINE('',#35338,#5797);
#4574=LINE('',#35342,#5798);
#4575=LINE('',#35344,#5799);
#4576=LINE('',#35348,#5800);
#4577=LINE('',#35350,#5801);
#4578=LINE('',#35354,#5802);
#4579=LINE('',#35356,#5803);
#4580=LINE('',#35360,#5804);
#4581=LINE('',#35362,#5805);
#4582=LINE('',#35366,#5806);
#4583=LINE('',#35368,#5807);
#4584=LINE('',#35372,#5808);
#4585=LINE('',#35374,#5809);
#4586=LINE('',#35378,#5810);
#4587=LINE('',#35380,#5811);
#4588=LINE('',#35384,#5812);
#4589=LINE('',#35386,#5813);
#4590=LINE('',#35390,#5814);
#4591=LINE('',#35392,#5815);
#4592=LINE('',#35396,#5816);
#4593=LINE('',#35398,#5817);
#4594=LINE('',#35402,#5818);
#4595=LINE('',#35404,#5819);
#4596=LINE('',#35408,#5820);
#4597=LINE('',#35410,#5821);
#4598=LINE('',#35414,#5822);
#4599=LINE('',#35416,#5823);
#4600=LINE('',#35420,#5824);
#4601=LINE('',#35422,#5825);
#4602=LINE('',#35426,#5826);
#4603=LINE('',#35428,#5827);
#4604=LINE('',#35432,#5828);
#4605=LINE('',#35434,#5829);
#4606=LINE('',#35438,#5830);
#4607=LINE('',#35440,#5831);
#4608=LINE('',#35444,#5832);
#4609=LINE('',#35446,#5833);
#4610=LINE('',#35450,#5834);
#4611=LINE('',#35452,#5835);
#4612=LINE('',#35456,#5836);
#4613=LINE('',#35458,#5837);
#4614=LINE('',#35462,#5838);
#4615=LINE('',#35464,#5839);
#4616=LINE('',#35468,#5840);
#4617=LINE('',#35470,#5841);
#4618=LINE('',#35474,#5842);
#4619=LINE('',#35476,#5843);
#4620=LINE('',#35480,#5844);
#4621=LINE('',#35482,#5845);
#4622=LINE('',#35486,#5846);
#4623=LINE('',#35488,#5847);
#4624=LINE('',#35492,#5848);
#4625=LINE('',#35494,#5849);
#4626=LINE('',#35498,#5850);
#4627=LINE('',#35500,#5851);
#4628=LINE('',#35504,#5852);
#4629=LINE('',#35506,#5853);
#4630=LINE('',#35510,#5854);
#4631=LINE('',#35512,#5855);
#4632=LINE('',#35516,#5856);
#4633=LINE('',#35518,#5857);
#4634=LINE('',#35523,#5858);
#4635=LINE('',#35527,#5859);
#4636=LINE('',#35531,#5860);
#4637=LINE('',#35535,#5861);
#4638=LINE('',#35539,#5862);
#4639=LINE('',#35542,#5863);
#4640=LINE('',#35547,#5864);
#4641=LINE('',#35605,#5865);
#4642=LINE('',#35607,#5866);
#4643=LINE('',#35608,#5867);
#4644=LINE('',#35611,#5868);
#4645=LINE('',#35612,#5869);
#4646=LINE('',#35615,#5870);
#4647=LINE('',#35616,#5871);
#4648=LINE('',#35619,#5872);
#4649=LINE('',#35620,#5873);
#4650=LINE('',#35623,#5874);
#4651=LINE('',#35624,#5875);
#4652=LINE('',#35627,#5876);
#4653=LINE('',#35628,#5877);
#4654=LINE('',#35631,#5878);
#4655=LINE('',#35632,#5879);
#4656=LINE('',#35635,#5880);
#4657=LINE('',#35636,#5881);
#4658=LINE('',#35639,#5882);
#4659=LINE('',#35640,#5883);
#4660=LINE('',#35642,#5884);
#4661=LINE('',#35644,#5885);
#4662=LINE('',#35647,#5886);
#4663=LINE('',#35650,#5887);
#4664=LINE('',#35651,#5888);
#4665=LINE('',#35653,#5889);
#4666=LINE('',#35655,#5890);
#4667=LINE('',#35658,#5891);
#4668=LINE('',#35659,#5892);
#4669=LINE('',#35661,#5893);
#4670=LINE('',#35665,#5894);
#4671=LINE('',#35675,#5895);
#4672=LINE('',#35676,#5896);
#4673=LINE('',#35682,#5897);
#4674=LINE('',#35689,#5898);
#4675=LINE('',#35690,#5899);
#4676=LINE('',#35696,#5900);
#4677=LINE('',#35703,#5901);
#4678=LINE('',#35704,#5902);
#4679=LINE('',#35710,#5903);
#4680=LINE('',#35717,#5904);
#4681=LINE('',#35718,#5905);
#4682=LINE('',#35724,#5906);
#4683=LINE('',#35731,#5907);
#4684=LINE('',#35732,#5908);
#4685=LINE('',#35738,#5909);
#4686=LINE('',#35745,#5910);
#4687=LINE('',#35746,#5911);
#4688=LINE('',#35752,#5912);
#4689=LINE('',#35759,#5913);
#4690=LINE('',#35760,#5914);
#4691=LINE('',#35766,#5915);
#4692=LINE('',#35773,#5916);
#4693=LINE('',#35774,#5917);
#4694=LINE('',#35780,#5918);
#4695=LINE('',#35787,#5919);
#4696=LINE('',#35788,#5920);
#4697=LINE('',#35794,#5921);
#4698=LINE('',#35801,#5922);
#4699=LINE('',#35802,#5923);
#4700=LINE('',#35808,#5924);
#4701=LINE('',#35815,#5925);
#4702=LINE('',#35816,#5926);
#4703=LINE('',#35822,#5927);
#4704=LINE('',#35829,#5928);
#4705=LINE('',#35830,#5929);
#4706=LINE('',#35836,#5930);
#4707=LINE('',#35843,#5931);
#4708=LINE('',#35844,#5932);
#4709=LINE('',#35850,#5933);
#4710=LINE('',#35857,#5934);
#4711=LINE('',#35858,#5935);
#4712=LINE('',#35864,#5936);
#4713=LINE('',#35871,#5937);
#4714=LINE('',#35872,#5938);
#4715=LINE('',#35878,#5939);
#4716=LINE('',#35885,#5940);
#4717=LINE('',#35886,#5941);
#4718=LINE('',#35892,#5942);
#4719=LINE('',#35899,#5943);
#4720=LINE('',#35900,#5944);
#4721=LINE('',#35906,#5945);
#4722=LINE('',#35913,#5946);
#4723=LINE('',#35914,#5947);
#4724=LINE('',#35920,#5948);
#4725=LINE('',#35927,#5949);
#4726=LINE('',#35928,#5950);
#4727=LINE('',#35934,#5951);
#4728=LINE('',#35941,#5952);
#4729=LINE('',#35942,#5953);
#4730=LINE('',#35948,#5954);
#4731=LINE('',#35955,#5955);
#4732=LINE('',#35956,#5956);
#4733=LINE('',#35962,#5957);
#4734=LINE('',#35969,#5958);
#4735=LINE('',#35970,#5959);
#4736=LINE('',#35976,#5960);
#4737=LINE('',#35983,#5961);
#4738=LINE('',#35984,#5962);
#4739=LINE('',#35990,#5963);
#4740=LINE('',#35997,#5964);
#4741=LINE('',#35998,#5965);
#4742=LINE('',#36004,#5966);
#4743=LINE('',#36011,#5967);
#4744=LINE('',#36012,#5968);
#4745=LINE('',#36018,#5969);
#4746=LINE('',#36025,#5970);
#4747=LINE('',#36026,#5971);
#4748=LINE('',#36032,#5972);
#4749=LINE('',#36039,#5973);
#4750=LINE('',#36040,#5974);
#4751=LINE('',#36046,#5975);
#4752=LINE('',#36053,#5976);
#4753=LINE('',#36054,#5977);
#4754=LINE('',#36060,#5978);
#4755=LINE('',#36067,#5979);
#4756=LINE('',#36068,#5980);
#4757=LINE('',#36074,#5981);
#4758=LINE('',#36081,#5982);
#4759=LINE('',#36082,#5983);
#4760=LINE('',#36088,#5984);
#4761=LINE('',#36095,#5985);
#4762=LINE('',#36096,#5986);
#4763=LINE('',#36102,#5987);
#4764=LINE('',#36109,#5988);
#4765=LINE('',#36110,#5989);
#4766=LINE('',#36116,#5990);
#4767=LINE('',#36123,#5991);
#4768=LINE('',#36124,#5992);
#4769=LINE('',#36130,#5993);
#4770=LINE('',#36137,#5994);
#4771=LINE('',#36138,#5995);
#4772=LINE('',#36144,#5996);
#4773=LINE('',#36151,#5997);
#4774=LINE('',#36152,#5998);
#4775=LINE('',#36158,#5999);
#4776=LINE('',#36165,#6000);
#4777=LINE('',#36166,#6001);
#4778=LINE('',#36172,#6002);
#4779=LINE('',#36249,#6003);
#4780=LINE('',#36253,#6004);
#4781=LINE('',#36259,#6005);
#4782=LINE('',#36283,#6006);
#4783=LINE('',#36331,#6007);
#4784=LINE('',#36379,#6008);
#4785=LINE('',#36433,#6009);
#4786=LINE('',#36481,#6010);
#4787=LINE('',#36529,#6011);
#4788=LINE('',#36583,#6012);
#4789=LINE('',#36631,#6013);
#4790=LINE('',#36679,#6014);
#4791=LINE('',#36727,#6015);
#4792=LINE('',#36781,#6016);
#4793=LINE('',#36799,#6017);
#4794=LINE('',#36824,#6018);
#4795=LINE('',#36849,#6019);
#4796=LINE('',#36873,#6020);
#4797=LINE('',#36897,#6021);
#4798=LINE('',#36922,#6022);
#4799=LINE('',#36947,#6023);
#4800=LINE('',#36971,#6024);
#4801=LINE('',#36996,#6025);
#4802=LINE('',#37021,#6026);
#4803=LINE('',#37925,#6027);
#4804=LINE('',#37930,#6028);
#4805=LINE('',#37937,#6029);
#4806=LINE('',#37948,#6030);
#4807=LINE('',#37953,#6031);
#4808=LINE('',#37960,#6032);
#4809=LINE('',#37971,#6033);
#4810=LINE('',#37976,#6034);
#4811=LINE('',#37983,#6035);
#4812=LINE('',#37994,#6036);
#4813=LINE('',#37999,#6037);
#4814=LINE('',#38006,#6038);
#4815=LINE('',#38017,#6039);
#4816=LINE('',#38022,#6040);
#4817=LINE('',#38029,#6041);
#4818=LINE('',#38040,#6042);
#4819=LINE('',#38045,#6043);
#4820=LINE('',#38052,#6044);
#4821=LINE('',#38063,#6045);
#4822=LINE('',#38068,#6046);
#4823=LINE('',#38075,#6047);
#4824=LINE('',#38086,#6048);
#4825=LINE('',#38091,#6049);
#4826=LINE('',#38098,#6050);
#4827=LINE('',#38109,#6051);
#4828=LINE('',#38114,#6052);
#4829=LINE('',#38121,#6053);
#4830=LINE('',#38132,#6054);
#4831=LINE('',#38137,#6055);
#4832=LINE('',#38144,#6056);
#4833=LINE('',#38155,#6057);
#4834=LINE('',#38160,#6058);
#4835=LINE('',#38167,#6059);
#4836=LINE('',#38178,#6060);
#4837=LINE('',#38183,#6061);
#4838=LINE('',#38190,#6062);
#4839=LINE('',#38201,#6063);
#4840=LINE('',#38206,#6064);
#4841=LINE('',#38213,#6065);
#4842=LINE('',#38224,#6066);
#4843=LINE('',#38229,#6067);
#4844=LINE('',#38236,#6068);
#4845=LINE('',#38247,#6069);
#4846=LINE('',#38252,#6070);
#4847=LINE('',#38259,#6071);
#4848=LINE('',#38270,#6072);
#4849=LINE('',#38275,#6073);
#4850=LINE('',#38282,#6074);
#4851=LINE('',#38293,#6075);
#4852=LINE('',#38298,#6076);
#4853=LINE('',#38305,#6077);
#4854=LINE('',#38316,#6078);
#4855=LINE('',#38321,#6079);
#4856=LINE('',#38328,#6080);
#4857=LINE('',#38339,#6081);
#4858=LINE('',#38344,#6082);
#4859=LINE('',#38351,#6083);
#4860=LINE('',#38362,#6084);
#4861=LINE('',#38367,#6085);
#4862=LINE('',#38374,#6086);
#4863=LINE('',#38385,#6087);
#4864=LINE('',#38390,#6088);
#4865=LINE('',#38397,#6089);
#4866=LINE('',#38408,#6090);
#4867=LINE('',#38413,#6091);
#4868=LINE('',#38420,#6092);
#4869=LINE('',#38431,#6093);
#4870=LINE('',#38436,#6094);
#4871=LINE('',#38443,#6095);
#4872=LINE('',#38454,#6096);
#4873=LINE('',#38459,#6097);
#4874=LINE('',#38466,#6098);
#4875=LINE('',#38544,#6099);
#4876=LINE('',#38550,#6100);
#4877=LINE('',#38557,#6101);
#4878=VECTOR('',#17811,1.);
#4879=VECTOR('',#17812,1.);
#4880=VECTOR('',#17813,1.);
#4881=VECTOR('',#17814,1.);
#4882=VECTOR('',#17815,1.);
#4883=VECTOR('',#17816,1.);
#4884=VECTOR('',#17819,1.);
#4885=VECTOR('',#17820,1.);
#4886=VECTOR('',#17821,1.);
#4887=VECTOR('',#17822,1.);
#4888=VECTOR('',#17825,1.);
#4889=VECTOR('',#17826,1.);
#4890=VECTOR('',#17827,1.);
#4891=VECTOR('',#17828,1.);
#4892=VECTOR('',#17831,1.);
#4893=VECTOR('',#17832,1.);
#4894=VECTOR('',#17835,1.);
#4895=VECTOR('',#17836,1.);
#4896=VECTOR('',#17837,1.);
#4897=VECTOR('',#17838,1.);
#4898=VECTOR('',#17841,1.);
#4899=VECTOR('',#17842,1.);
#4900=VECTOR('',#17843,1.);
#4901=VECTOR('',#17846,1.);
#4902=VECTOR('',#17847,1.);
#4903=VECTOR('',#17848,1.);
#4904=VECTOR('',#17849,1.);
#4905=VECTOR('',#17850,1.);
#4906=VECTOR('',#17851,1.);
#4907=VECTOR('',#17854,1.);
#4908=VECTOR('',#17855,1.);
#4909=VECTOR('',#17856,1.);
#4910=VECTOR('',#17859,1.);
#4911=VECTOR('',#17860,1.);
#4912=VECTOR('',#17861,1.);
#4913=VECTOR('',#17864,1.);
#4914=VECTOR('',#17865,1.);
#4915=VECTOR('',#17866,1.);
#4916=VECTOR('',#17869,1.);
#4917=VECTOR('',#17870,1.);
#4918=VECTOR('',#17871,1.);
#4919=VECTOR('',#17872,1.);
#4920=VECTOR('',#17873,1.);
#4921=VECTOR('',#17874,1.);
#4922=VECTOR('',#17877,1.);
#4923=VECTOR('',#17878,1.);
#4924=VECTOR('',#17879,1.);
#4925=VECTOR('',#17880,1.);
#4926=VECTOR('',#17883,1.);
#4927=VECTOR('',#17884,1.);
#4928=VECTOR('',#17887,1.);
#4929=VECTOR('',#17888,1.);
#4930=VECTOR('',#17889,1.);
#4931=VECTOR('',#17892,1.);
#4932=VECTOR('',#17893,1.);
#4933=VECTOR('',#17894,1.);
#4934=VECTOR('',#17895,1.);
#4935=VECTOR('',#17896,1.);
#4936=VECTOR('',#17897,1.);
#4937=VECTOR('',#17900,1.);
#4938=VECTOR('',#17901,1.);
#4939=VECTOR('',#17902,1.);
#4940=VECTOR('',#17903,1.);
#4941=VECTOR('',#17904,1.);
#4942=VECTOR('',#17907,1.);
#4943=VECTOR('',#17908,1.);
#4944=VECTOR('',#17911,1.);
#4945=VECTOR('',#17912,1.);
#4946=VECTOR('',#17913,1.);
#4947=VECTOR('',#17914,1.);
#4948=VECTOR('',#17917,1.);
#4949=VECTOR('',#17918,1.);
#4950=VECTOR('',#17919,1.);
#4951=VECTOR('',#17924,1.0543933982822);
#4952=VECTOR('',#17929,1.025);
#4953=VECTOR('',#17938,1.0106066017178);
#4954=VECTOR('',#17943,1.);
#4955=VECTOR('',#17946,1.);
#4956=VECTOR('',#17949,0.205);
#4957=VECTOR('',#17952,1.);
#4958=VECTOR('',#17953,1.);
#4959=VECTOR('',#17954,1.);
#4960=VECTOR('',#17955,1.);
#4961=VECTOR('',#17956,1.);
#4962=VECTOR('',#17957,1.);
#4963=VECTOR('',#17960,1.);
#4964=VECTOR('',#17961,1.);
#4965=VECTOR('',#17962,1.);
#4966=VECTOR('',#17965,1.);
#4967=VECTOR('',#17966,1.);
#4968=VECTOR('',#17967,1.);
#4969=VECTOR('',#17968,1.);
#4970=VECTOR('',#17971,1.);
#4971=VECTOR('',#17972,1.);
#4972=VECTOR('',#17973,1.);
#4973=VECTOR('',#17976,1.);
#4974=VECTOR('',#17977,1.);
#4975=VECTOR('',#17978,1.);
#4976=VECTOR('',#17979,1.);
#4977=VECTOR('',#17980,1.);
#4978=VECTOR('',#17981,1.);
#4979=VECTOR('',#17984,1.);
#4980=VECTOR('',#17985,1.);
#4981=VECTOR('',#17986,1.);
#4982=VECTOR('',#17987,1.);
#4983=VECTOR('',#17990,1.);
#4984=VECTOR('',#17991,1.);
#4985=VECTOR('',#17994,1.);
#4986=VECTOR('',#17995,1.);
#4987=VECTOR('',#17996,1.);
#4988=VECTOR('',#17999,1.);
#4989=VECTOR('',#18006,1.);
#4990=VECTOR('',#18007,1.);
#4991=VECTOR('',#18008,1.);
#4992=VECTOR('',#18017,1.);
#4993=VECTOR('',#18018,1.);
#4994=VECTOR('',#18019,1.);
#4995=VECTOR('',#18020,1.);
#4996=VECTOR('',#18023,1.);
#4997=VECTOR('',#18024,1.);
#4998=VECTOR('',#18027,1.);
#4999=VECTOR('',#18032,1.);
#5000=VECTOR('',#18033,1.);
#5001=VECTOR('',#18036,1.);
#5002=VECTOR('',#18041,1.);
#5003=VECTOR('',#18044,1.);
#5004=VECTOR('',#18045,1.);
#5005=VECTOR('',#18046,1.);
#5006=VECTOR('',#18047,1.);
#5007=VECTOR('',#18050,1.);
#5008=VECTOR('',#18057,1.);
#5009=VECTOR('',#18058,1.);
#5010=VECTOR('',#18059,1.);
#5011=VECTOR('',#18062,1.);
#5012=VECTOR('',#18069,1.);
#5013=VECTOR('',#18070,1.);
#5014=VECTOR('',#18071,1.);
#5015=VECTOR('',#18074,1.);
#5016=VECTOR('',#18077,1.);
#5017=VECTOR('',#18080,1.);
#5018=VECTOR('',#18083,1.);
#5019=VECTOR('',#18088,1.);
#5020=VECTOR('',#18089,1.);
#5021=VECTOR('',#18092,1.);
#5022=VECTOR('',#18099,1.);
#5023=VECTOR('',#18100,1.);
#5024=VECTOR('',#18103,1.);
#5025=VECTOR('',#18104,1.);
#5026=VECTOR('',#18107,1.);
#5027=VECTOR('',#18108,1.);
#5028=VECTOR('',#18111,1.);
#5029=VECTOR('',#18118,1.);
#5030=VECTOR('',#18119,1.);
#5031=VECTOR('',#18122,1.);
#5032=VECTOR('',#18123,1.);
#5033=VECTOR('',#18126,1.);
#5034=VECTOR('',#18133,1.);
#5035=VECTOR('',#18134,1.);
#5036=VECTOR('',#18135,1.);
#5037=VECTOR('',#18138,1.);
#5038=VECTOR('',#18145,1.);
#5039=VECTOR('',#18146,1.);
#5040=VECTOR('',#18149,1.);
#5041=VECTOR('',#18150,1.);
#5042=VECTOR('',#18151,1.);
#5043=VECTOR('',#18154,1.);
#5044=VECTOR('',#18161,1.);
#5045=VECTOR('',#18162,1.);
#5046=VECTOR('',#18163,1.);
#5047=VECTOR('',#18166,1.);
#5048=VECTOR('',#18167,1.);
#5049=VECTOR('',#18170,1.);
#5050=VECTOR('',#18171,1.);
#5051=VECTOR('',#18172,1.);
#5052=VECTOR('',#18175,1.);
#5053=VECTOR('',#18182,1.);
#5054=VECTOR('',#18187,1.);
#5055=VECTOR('',#18192,1.6);
#5056=VECTOR('',#18201,1.5893933982822);
#5057=VECTOR('',#18204,1.57);
#5058=VECTOR('',#18213,1.);
#5059=VECTOR('',#18214,1.);
#5060=VECTOR('',#18215,1.);
#5061=VECTOR('',#18218,1.);
#5062=VECTOR('',#18219,1.);
#5063=VECTOR('',#18220,1.);
#5064=VECTOR('',#18223,1.);
#5065=VECTOR('',#18230,1.);
#5066=VECTOR('',#18231,1.);
#5067=VECTOR('',#18232,1.);
#5068=VECTOR('',#18235,1.);
#5069=VECTOR('',#18242,1.);
#5070=VECTOR('',#18243,1.);
#5071=VECTOR('',#18246,1.);
#5072=VECTOR('',#18247,1.);
#5073=VECTOR('',#18248,1.);
#5074=VECTOR('',#18251,1.);
#5075=VECTOR('',#18258,1.);
#5076=VECTOR('',#18259,1.);
#5077=VECTOR('',#18262,1.);
#5078=VECTOR('',#18263,1.);
#5079=VECTOR('',#18264,1.);
#5080=VECTOR('',#18267,1.);
#5081=VECTOR('',#18274,1.);
#5082=VECTOR('',#18275,1.);
#5083=VECTOR('',#18278,1.);
#5084=VECTOR('',#18279,1.);
#5085=VECTOR('',#18280,1.);
#5086=VECTOR('',#18283,1.);
#5087=VECTOR('',#18290,1.);
#5088=VECTOR('',#18293,1.);
#5089=VECTOR('',#18294,1.);
#5090=VECTOR('',#18297,1.);
#5091=VECTOR('',#18304,1.);
#5092=VECTOR('',#18305,1.);
#5093=VECTOR('',#18308,1.);
#5094=VECTOR('',#18313,1.);
#5095=VECTOR('',#18314,1.);
#5096=VECTOR('',#18321,1.);
#5097=VECTOR('',#18326,1.);
#5098=VECTOR('',#18329,1.);
#5099=VECTOR('',#18330,1.);
#5100=VECTOR('',#18333,1.);
#5101=VECTOR('',#18338,1.);
#5102=VECTOR('',#18345,1.);
#5103=VECTOR('',#18348,1.);
#5104=VECTOR('',#18349,1.);
#5105=VECTOR('',#18356,1.);
#5106=VECTOR('',#18359,1.);
#5107=VECTOR('',#18368,1.);
#5108=VECTOR('',#18377,1.);
#5109=VECTOR('',#18380,1.);
#5110=VECTOR('',#18385,1.);
#5111=VECTOR('',#18390,1.);
#5112=VECTOR('',#18393,1.);
#5113=VECTOR('',#18408,0.2175);
#5114=VECTOR('',#18413,0.205);
#5115=VECTOR('',#18420,0.435);
#5116=VECTOR('',#18429,0.205);
#5117=VECTOR('',#18432,1.);
#5118=VECTOR('',#18435,1.);
#5119=VECTOR('',#18438,0.205);
#5120=VECTOR('',#18441,1.);
#5121=VECTOR('',#18446,0.205);
#5122=VECTOR('',#18451,1.);
#5123=VECTOR('',#18460,0.975);
#5124=VECTOR('',#18465,1.);
#5125=VECTOR('',#18474,1.275);
#5126=VECTOR('',#18479,1.3);
#5127=VECTOR('',#18480,1.3);
#5128=VECTOR('',#18485,1.27);
#5129=VECTOR('',#18492,0.73);
#5130=VECTOR('',#18497,0.705);
#5131=VECTOR('',#18498,0.705);
#5132=VECTOR('',#18509,0.645606601717798);
#5133=VECTOR('',#18516,0.675);
#5134=VECTOR('',#18525,0.689393398282202);
#5135=VECTOR('',#18532,0.7);
#5136=VECTOR('',#18539,0.689393398282202);
#5137=VECTOR('',#18546,0.675);
#5138=VECTOR('',#18553,0.645606601717798);
#5139=VECTOR('',#18562,1.);
#5140=VECTOR('',#18563,1.);
#5141=VECTOR('',#18564,1.);
#5142=VECTOR('',#18565,1.);
#5143=VECTOR('',#18566,1.);
#5144=VECTOR('',#18567,1.);
#5145=VECTOR('',#18570,1.);
#5146=VECTOR('',#18571,1.);
#5147=VECTOR('',#18572,1.);
#5148=VECTOR('',#18573,1.);
#5149=VECTOR('',#18574,1.);
#5150=VECTOR('',#18577,1.);
#5151=VECTOR('',#18578,1.);
#5152=VECTOR('',#18579,1.);
#5153=VECTOR('',#18580,1.);
#5154=VECTOR('',#18581,1.);
#5155=VECTOR('',#18582,1.);
#5156=VECTOR('',#18583,1.);
#5157=VECTOR('',#18586,1.);
#5158=VECTOR('',#18587,1.);
#5159=VECTOR('',#18590,1.);
#5160=VECTOR('',#18591,1.);
#5161=VECTOR('',#18592,1.);
#5162=VECTOR('',#18593,1.);
#5163=VECTOR('',#18594,1.);
#5164=VECTOR('',#18597,1.);
#5165=VECTOR('',#18600,1.);
#5166=VECTOR('',#18601,1.);
#5167=VECTOR('',#18602,1.);
#5168=VECTOR('',#18603,1.);
#5169=VECTOR('',#18604,1.);
#5170=VECTOR('',#18605,1.);
#5171=VECTOR('',#18608,1.);
#5172=VECTOR('',#18609,1.);
#5173=VECTOR('',#18610,1.);
#5174=VECTOR('',#18613,1.);
#5175=VECTOR('',#18614,1.);
#5176=VECTOR('',#18615,1.);
#5177=VECTOR('',#18616,1.);
#5178=VECTOR('',#18617,1.);
#5179=VECTOR('',#18618,1.);
#5180=VECTOR('',#18621,1.);
#5181=VECTOR('',#18622,1.);
#5182=VECTOR('',#18623,1.);
#5183=VECTOR('',#18624,1.);
#5184=VECTOR('',#18625,1.);
#5185=VECTOR('',#18628,1.);
#5186=VECTOR('',#18629,1.);
#5187=VECTOR('',#18630,1.);
#5188=VECTOR('',#18631,1.);
#5189=VECTOR('',#18632,1.);
#5190=VECTOR('',#18635,1.);
#5191=VECTOR('',#18636,1.);
#5192=VECTOR('',#18639,1.);
#5193=VECTOR('',#18640,1.);
#5194=VECTOR('',#18641,1.);
#5195=VECTOR('',#18644,1.);
#5196=VECTOR('',#18645,1.);
#5197=VECTOR('',#18648,1.);
#5198=VECTOR('',#18649,1.);
#5199=VECTOR('',#18650,1.);
#5200=VECTOR('',#18651,1.);
#5201=VECTOR('',#18652,1.);
#5202=VECTOR('',#18653,1.);
#5203=VECTOR('',#18656,1.);
#5204=VECTOR('',#18657,1.);
#5205=VECTOR('',#18658,1.);
#5206=VECTOR('',#18659,1.);
#5207=VECTOR('',#18660,1.);
#5208=VECTOR('',#18663,1.);
#5209=VECTOR('',#18664,1.);
#5210=VECTOR('',#18665,1.);
#5211=VECTOR('',#18666,1.);
#5212=VECTOR('',#18667,1.);
#5213=VECTOR('',#18670,1.);
#5214=VECTOR('',#18671,1.);
#5215=VECTOR('',#18674,1.);
#5216=VECTOR('',#18675,1.);
#5217=VECTOR('',#18676,1.);
#5218=VECTOR('',#18679,1.);
#5219=VECTOR('',#18680,1.);
#5220=VECTOR('',#18681,1.);
#5221=VECTOR('',#18684,1.);
#5222=VECTOR('',#18685,1.);
#5223=VECTOR('',#18686,1.);
#5224=VECTOR('',#18687,1.);
#5225=VECTOR('',#18688,1.);
#5226=VECTOR('',#18691,1.);
#5227=VECTOR('',#18692,1.);
#5228=VECTOR('',#18693,1.);
#5229=VECTOR('',#18694,1.);
#5230=VECTOR('',#18695,1.);
#5231=VECTOR('',#18696,1.);
#5232=VECTOR('',#18697,1.);
#5233=VECTOR('',#18700,1.);
#5234=VECTOR('',#18701,1.);
#5235=VECTOR('',#18704,1.);
#5236=VECTOR('',#18705,1.);
#5237=VECTOR('',#18706,1.);
#5238=VECTOR('',#18707,1.);
#5239=VECTOR('',#18708,1.);
#5240=VECTOR('',#18711,1.);
#5241=VECTOR('',#18712,1.);
#5242=VECTOR('',#18713,1.);
#5243=VECTOR('',#18714,1.);
#5244=VECTOR('',#18717,1.);
#5245=VECTOR('',#18718,1.);
#5246=VECTOR('',#18721,1.);
#5247=VECTOR('',#18724,1.);
#5248=VECTOR('',#18725,1.);
#5249=VECTOR('',#18726,1.);
#5250=VECTOR('',#18729,1.);
#5251=VECTOR('',#18730,1.);
#5252=VECTOR('',#18735,1.);
#5253=VECTOR('',#18736,1.);
#5254=VECTOR('',#18737,1.);
#5255=VECTOR('',#18738,1.);
#5256=VECTOR('',#18741,1.);
#5257=VECTOR('',#18742,1.);
#5258=VECTOR('',#18747,1.);
#5259=VECTOR('',#18748,1.);
#5260=VECTOR('',#18751,1.);
#5261=VECTOR('',#18768,1.);
#5262=VECTOR('',#18771,1.);
#5263=VECTOR('',#18772,1.);
#5264=VECTOR('',#18775,1.);
#5265=VECTOR('',#18776,1.);
#5266=VECTOR('',#18779,1.);
#5267=VECTOR('',#18780,1.);
#5268=VECTOR('',#18781,1.);
#5269=VECTOR('',#18788,1.1106066017178);
#5270=VECTOR('',#18799,1.1);
#5271=VECTOR('',#18802,1.14);
#5272=VECTOR('',#18809,1.115);
#5273=VECTOR('',#18818,1.275);
#5274=VECTOR('',#18829,1.26);
#5275=VECTOR('',#18832,1.37);
#5276=VECTOR('',#18837,1.355);
#5277=VECTOR('',#18840,0.239999999999999);
#5278=VECTOR('',#18849,0.225);
#5279=VECTOR('',#18854,0.239999999999999);
#5280=VECTOR('',#18861,0.240000000000001);
#5281=VECTOR('',#18870,0.225000000000001);
#5282=VECTOR('',#18875,0.240000000000001);
#5283=VECTOR('',#18882,0.27);
#5284=VECTOR('',#18889,0.255);
#5285=VECTOR('',#18892,0.27);
#5286=VECTOR('',#18899,0.255000000000001);
#5287=VECTOR('',#18902,0.27);
#5288=VECTOR('',#18909,0.255);
#5289=VECTOR('',#18914,0.415);
#5290=VECTOR('',#18919,1.);
#5291=VECTOR('',#18920,1.);
#5292=VECTOR('',#18921,1.);
#5293=VECTOR('',#18922,1.);
#5294=VECTOR('',#18935,0.4);
#5295=VECTOR('',#18938,0.415);
#5296=VECTOR('',#18943,0.4);
#5297=VECTOR('',#18946,1.1543933982822);
#5298=VECTOR('',#18949,1.);
#5299=VECTOR('',#18950,1.);
#5300=VECTOR('',#18953,1.);
#5301=VECTOR('',#18956,1.);
#5302=VECTOR('',#18961,0.27);
#5303=VECTOR('',#18964,0.27);
#5304=VECTOR('',#18967,0.27);
#5305=VECTOR('',#18984,1.235);
#5306=VECTOR('',#18989,1.25);
#5307=VECTOR('',#18994,1.235);
#5308=VECTOR('',#19001,1.35);
#5309=VECTOR('',#19002,1.);
#5310=VECTOR('',#19005,1.35);
#5311=VECTOR('',#19008,1.286875);
#5312=VECTOR('',#19013,1.286875);
#5313=VECTOR('',#19018,1.);
#5314=VECTOR('',#19023,1.);
#5315=VECTOR('',#19026,1.);
#5316=VECTOR('',#19031,1.);
#5317=VECTOR('',#19036,1.);
#5318=VECTOR('',#19037,1.);
#5319=VECTOR('',#19042,1.);
#5320=VECTOR('',#19051,1.);
#5321=VECTOR('',#19052,1.);
#5322=VECTOR('',#19053,1.);
#5323=VECTOR('',#19056,1.);
#5324=VECTOR('',#19057,1.);
#5325=VECTOR('',#19058,1.);
#5326=VECTOR('',#19065,1.);
#5327=VECTOR('',#19070,1.);
#5328=VECTOR('',#19077,1.);
#5329=VECTOR('',#19078,1.);
#5330=VECTOR('',#19083,1.);
#5331=VECTOR('',#19086,1.);
#5332=VECTOR('',#19087,1.);
#5333=VECTOR('',#19092,1.05);
#5334=VECTOR('',#19121,1.335);
#5335=VECTOR('',#19128,0.2);
#5336=VECTOR('',#19133,0.2);
#5337=VECTOR('',#19136,0.2);
#5338=VECTOR('',#19139,0.2);
#5339=VECTOR('',#19142,0.2);
#5340=VECTOR('',#19145,0.2);
#5341=VECTOR('',#19148,0.15555);
#5342=VECTOR('',#19153,0.15555);
#5343=VECTOR('',#19156,0.15555);
#5344=VECTOR('',#19159,0.15555);
#5345=VECTOR('',#19162,0.15555);
#5346=VECTOR('',#19165,0.15555);
#5347=VECTOR('',#19184,1.);
#5348=VECTOR('',#19189,1.);
#5349=VECTOR('',#19194,1.);
#5350=VECTOR('',#19199,1.);
#5351=VECTOR('',#19204,1.);
#5352=VECTOR('',#19209,1.);
#5353=VECTOR('',#19214,0.0577350269189626);
#5354=VECTOR('',#19231,1.);
#5355=VECTOR('',#19232,1.);
#5356=VECTOR('',#19233,1.);
#5357=VECTOR('',#19236,1.);
#5358=VECTOR('',#19237,1.);
#5359=VECTOR('',#19240,1.);
#5360=VECTOR('',#19241,1.);
#5361=VECTOR('',#19244,1.);
#5362=VECTOR('',#19245,1.);
#5363=VECTOR('',#19248,1.);
#5364=VECTOR('',#19249,1.);
#5365=VECTOR('',#19252,1.);
#5366=VECTOR('',#19253,1.);
#5367=VECTOR('',#19256,1.);
#5368=VECTOR('',#19257,1.);
#5369=VECTOR('',#19260,1.);
#5370=VECTOR('',#19261,1.);
#5371=VECTOR('',#19264,1.);
#5372=VECTOR('',#19265,1.);
#5373=VECTOR('',#19268,1.);
#5374=VECTOR('',#19271,1.);
#5375=VECTOR('',#19276,1.);
#5376=VECTOR('',#19279,1.);
#5377=VECTOR('',#19280,1.);
#5378=VECTOR('',#19283,1.);
#5379=VECTOR('',#19286,1.);
#5380=VECTOR('',#19289,1.);
#5381=VECTOR('',#19290,1.);
#5382=VECTOR('',#19293,1.);
#5383=VECTOR('',#19300,1.);
#5384=VECTOR('',#19313,0.1625);
#5385=VECTOR('',#19322,0.185);
#5386=VECTOR('',#19329,0.2);
#5387=VECTOR('',#19334,0.2);
#5388=VECTOR('',#19337,0.2);
#5389=VECTOR('',#19340,0.2);
#5390=VECTOR('',#19343,0.2);
#5391=VECTOR('',#19346,0.15555);
#5392=VECTOR('',#19351,0.15555);
#5393=VECTOR('',#19356,0.15555);
#5394=VECTOR('',#19359,0.15555);
#5395=VECTOR('',#19362,0.15555);
#5396=VECTOR('',#19381,1.);
#5397=VECTOR('',#19386,1.);
#5398=VECTOR('',#19391,1.);
#5399=VECTOR('',#19396,1.);
#5400=VECTOR('',#19401,1.);
#5401=VECTOR('',#19406,1.);
#5402=VECTOR('',#19411,0.0577350269189626);
#5403=VECTOR('',#19428,1.);
#5404=VECTOR('',#19429,1.);
#5405=VECTOR('',#19430,1.);
#5406=VECTOR('',#19433,1.);
#5407=VECTOR('',#19434,1.);
#5408=VECTOR('',#19437,1.);
#5409=VECTOR('',#19438,1.);
#5410=VECTOR('',#19441,1.);
#5411=VECTOR('',#19442,1.);
#5412=VECTOR('',#19445,1.);
#5413=VECTOR('',#19446,1.);
#5414=VECTOR('',#19449,1.);
#5415=VECTOR('',#19450,1.);
#5416=VECTOR('',#19453,1.);
#5417=VECTOR('',#19454,1.);
#5418=VECTOR('',#19457,1.);
#5419=VECTOR('',#19458,1.);
#5420=VECTOR('',#19461,1.);
#5421=VECTOR('',#19462,1.);
#5422=VECTOR('',#19465,1.);
#5423=VECTOR('',#19468,1.);
#5424=VECTOR('',#19473,1.);
#5425=VECTOR('',#19476,1.);
#5426=VECTOR('',#19477,1.);
#5427=VECTOR('',#19480,1.);
#5428=VECTOR('',#19483,1.);
#5429=VECTOR('',#19486,1.);
#5430=VECTOR('',#19487,1.);
#5431=VECTOR('',#19490,1.);
#5432=VECTOR('',#19497,1.);
#5433=VECTOR('',#19510,0.1625);
#5434=VECTOR('',#19519,0.185);
#5435=VECTOR('',#19526,1.);
#5436=VECTOR('',#19527,1.);
#5437=VECTOR('',#19528,1.);
#5438=VECTOR('',#19529,1.);
#5439=VECTOR('',#19530,1.);
#5440=VECTOR('',#19531,1.);
#5441=VECTOR('',#19534,1.);
#5442=VECTOR('',#19535,1.);
#5443=VECTOR('',#19536,1.);
#5444=VECTOR('',#19537,1.);
#5445=VECTOR('',#19540,1.);
#5446=VECTOR('',#19541,1.);
#5447=VECTOR('',#19542,1.);
#5448=VECTOR('',#19545,1.);
#5449=VECTOR('',#19546,1.);
#5450=VECTOR('',#19547,1.);
#5451=VECTOR('',#19550,1.);
#5452=VECTOR('',#19551,1.);
#5453=VECTOR('',#19552,1.);
#5454=VECTOR('',#19553,1.);
#5455=VECTOR('',#19556,1.);
#5456=VECTOR('',#19557,1.);
#5457=VECTOR('',#19558,1.);
#5458=VECTOR('',#19561,1.);
#5459=VECTOR('',#19562,1.);
#5460=VECTOR('',#19563,1.);
#5461=VECTOR('',#19566,1.);
#5462=VECTOR('',#19571,1.);
#5463=VECTOR('',#19572,1.);
#5464=VECTOR('',#19577,1.2);
#5465=VECTOR('',#19586,0.204999999999999);
#5466=VECTOR('',#19595,1.1893933982822);
#5467=VECTOR('',#19600,1.175);
#5468=VECTOR('',#19601,1.);
#5469=VECTOR('',#19606,0.7);
#5470=VECTOR('',#19611,1.1456066017178);
#5471=VECTOR('',#19620,1.);
#5472=VECTOR('',#19621,1.);
#5473=VECTOR('',#19622,1.);
#5474=VECTOR('',#19623,1.);
#5475=VECTOR('',#19626,1.);
#5476=VECTOR('',#19627,1.);
#5477=VECTOR('',#19628,1.);
#5478=VECTOR('',#19631,1.);
#5479=VECTOR('',#19632,1.);
#5480=VECTOR('',#19635,1.);
#5481=VECTOR('',#19636,1.);
#5482=VECTOR('',#19639,1.);
#5483=VECTOR('',#19640,1.);
#5484=VECTOR('',#19641,1.);
#5485=VECTOR('',#19646,1.);
#5486=VECTOR('',#19647,1.);
#5487=VECTOR('',#19648,1.);
#5488=VECTOR('',#19649,1.);
#5489=VECTOR('',#19650,1.);
#5490=VECTOR('',#19651,1.);
#5491=VECTOR('',#19654,1.);
#5492=VECTOR('',#19655,1.);
#5493=VECTOR('',#19656,1.);
#5494=VECTOR('',#19657,1.);
#5495=VECTOR('',#19658,1.);
#5496=VECTOR('',#19661,1.);
#5497=VECTOR('',#19662,1.);
#5498=VECTOR('',#19663,1.);
#5499=VECTOR('',#19664,1.);
#5500=VECTOR('',#19667,1.);
#5501=VECTOR('',#19668,1.);
#5502=VECTOR('',#19671,1.);
#5503=VECTOR('',#19672,1.);
#5504=VECTOR('',#19673,1.);
#5505=VECTOR('',#19676,1.);
#5506=VECTOR('',#19677,1.);
#5507=VECTOR('',#19678,1.);
#5508=VECTOR('',#19679,1.);
#5509=VECTOR('',#19680,1.);
#5510=VECTOR('',#19683,1.);
#5511=VECTOR('',#19684,1.);
#5512=VECTOR('',#19685,1.);
#5513=VECTOR('',#19688,1.);
#5514=VECTOR('',#19691,1.);
#5515=VECTOR('',#19692,1.);
#5516=VECTOR('',#19693,1.);
#5517=VECTOR('',#19694,1.);
#5518=VECTOR('',#19697,1.);
#5519=VECTOR('',#19698,1.);
#5520=VECTOR('',#19701,1.);
#5521=VECTOR('',#19702,1.);
#5522=VECTOR('',#19703,1.);
#5523=VECTOR('',#19704,1.);
#5524=VECTOR('',#19705,1.);
#5525=VECTOR('',#19706,1.);
#5526=VECTOR('',#19709,1.);
#5527=VECTOR('',#19712,1.);
#5528=VECTOR('',#19713,1.);
#5529=VECTOR('',#19716,1.);
#5530=VECTOR('',#19717,1.);
#5531=VECTOR('',#19720,1.);
#5532=VECTOR('',#19721,1.);
#5533=VECTOR('',#19724,1.);
#5534=VECTOR('',#19725,1.);
#5535=VECTOR('',#19726,1.);
#5536=VECTOR('',#19729,1.);
#5537=VECTOR('',#19730,1.);
#5538=VECTOR('',#19731,1.);
#5539=VECTOR('',#19732,1.);
#5540=VECTOR('',#19735,1.);
#5541=VECTOR('',#19736,1.);
#5542=VECTOR('',#19737,1.);
#5543=VECTOR('',#19738,1.);
#5544=VECTOR('',#19741,1.);
#5545=VECTOR('',#19742,1.);
#5546=VECTOR('',#19743,1.);
#5547=VECTOR('',#19744,1.);
#5548=VECTOR('',#19747,1.);
#5549=VECTOR('',#19748,1.);
#5550=VECTOR('',#19749,1.);
#5551=VECTOR('',#19750,1.);
#5552=VECTOR('',#19753,1.);
#5553=VECTOR('',#19754,1.);
#5554=VECTOR('',#19757,1.);
#5555=VECTOR('',#19758,1.);
#5556=VECTOR('',#19761,1.);
#5557=VECTOR('',#19762,1.);
#5558=VECTOR('',#19773,0.184393398282202);
#5559=VECTOR('',#19778,0.115);
#5560=VECTOR('',#19781,0.22);
#5561=VECTOR('',#19786,0.205);
#5562=VECTOR('',#19791,0.22);
#5563=VECTOR('',#19796,0.205);
#5564=VECTOR('',#19817,1.5543933982822);
#5565=VECTOR('',#19820,1.525);
#5566=VECTOR('',#19827,0.22);
#5567=VECTOR('',#19830,1.);
#5568=VECTOR('',#19831,1.);
#5569=VECTOR('',#19832,1.);
#5570=VECTOR('',#19833,1.);
#5571=VECTOR('',#19840,0.22);
#5572=VECTOR('',#19843,1.);
#5573=VECTOR('',#19844,1.);
#5574=VECTOR('',#19845,1.);
#5575=VECTOR('',#19848,1.);
#5576=VECTOR('',#19849,1.);
#5577=VECTOR('',#19850,1.);
#5578=VECTOR('',#19857,1.);
#5579=VECTOR('',#19858,1.);
#5580=VECTOR('',#19861,1.5106066017178);
#5581=VECTOR('',#19868,1.5);
#5582=VECTOR('',#19873,1.5543933982822);
#5583=VECTOR('',#19876,1.525);
#5584=VECTOR('',#19881,1.5106066017178);
#5585=VECTOR('',#19884,1.);
#5586=VECTOR('',#19889,0.72);
#5587=VECTOR('',#19896,1.);
#5588=VECTOR('',#19903,1.);
#5589=VECTOR('',#19910,0.25);
#5590=VECTOR('',#19915,0.25);
#5591=VECTOR('',#19918,0.25);
#5592=VECTOR('',#19921,0.25);
#5593=VECTOR('',#19924,0.25);
#5594=VECTOR('',#19927,0.25);
#5595=VECTOR('',#19930,0.25);
#5596=VECTOR('',#19933,0.25);
#5597=VECTOR('',#19936,0.25);
#5598=VECTOR('',#19939,0.25);
#5599=VECTOR('',#19942,0.25);
#5600=VECTOR('',#19945,0.25);
#5601=VECTOR('',#19948,0.25);
#5602=VECTOR('',#19951,0.25);
#5603=VECTOR('',#19954,0.25);
#5604=VECTOR('',#19957,0.25);
#5605=VECTOR('',#19960,0.25);
#5606=VECTOR('',#19963,0.25);
#5607=VECTOR('',#19966,0.25);
#5608=VECTOR('',#19969,0.25);
#5609=VECTOR('',#19972,0.25);
#5610=VECTOR('',#19975,0.25);
#5611=VECTOR('',#19978,0.25);
#5612=VECTOR('',#19981,0.25);
#5613=VECTOR('',#19986,0.217775);
#5614=VECTOR('',#19991,0.217775);
#5615=VECTOR('',#19994,0.217775);
#5616=VECTOR('',#19997,0.217775);
#5617=VECTOR('',#20000,0.217775);
#5618=VECTOR('',#20003,0.217775);
#5619=VECTOR('',#20006,0.217775);
#5620=VECTOR('',#20009,0.217775);
#5621=VECTOR('',#20012,0.217775);
#5622=VECTOR('',#20015,0.217775);
#5623=VECTOR('',#20018,0.217775);
#5624=VECTOR('',#20021,0.217775);
#5625=VECTOR('',#20024,0.217775);
#5626=VECTOR('',#20027,0.217775);
#5627=VECTOR('',#20030,0.217775);
#5628=VECTOR('',#20033,0.217775);
#5629=VECTOR('',#20036,0.217775);
#5630=VECTOR('',#20039,0.217775);
#5631=VECTOR('',#20042,0.217775);
#5632=VECTOR('',#20045,0.217775);
#5633=VECTOR('',#20048,0.217775);
#5634=VECTOR('',#20051,0.217775);
#5635=VECTOR('',#20054,0.217775);
#5636=VECTOR('',#20057,1.);
#5637=VECTOR('',#20058,1.);
#5638=VECTOR('',#20059,1.);
#5639=VECTOR('',#20060,1.);
#5640=VECTOR('',#20063,1.);
#5641=VECTOR('',#20064,1.);
#5642=VECTOR('',#20065,1.);
#5643=VECTOR('',#20068,1.);
#5644=VECTOR('',#20069,1.);
#5645=VECTOR('',#20070,1.);
#5646=VECTOR('',#20073,1.);
#5647=VECTOR('',#20074,1.);
#5648=VECTOR('',#20081,0.151);
#5649=VECTOR('',#20098,1.);
#5650=VECTOR('',#20099,1.);
#5651=VECTOR('',#20102,1.);
#5652=VECTOR('',#20105,1.);
#5653=VECTOR('',#20106,1.);
#5654=VECTOR('',#20109,1.);
#5655=VECTOR('',#20112,1.);
#5656=VECTOR('',#20113,1.);
#5657=VECTOR('',#20116,1.);
#5658=VECTOR('',#20119,1.);
#5659=VECTOR('',#20120,1.);
#5660=VECTOR('',#20123,1.);
#5661=VECTOR('',#20126,1.);
#5662=VECTOR('',#20127,1.);
#5663=VECTOR('',#20130,1.);
#5664=VECTOR('',#20133,1.);
#5665=VECTOR('',#20134,1.);
#5666=VECTOR('',#20137,1.);
#5667=VECTOR('',#20140,1.);
#5668=VECTOR('',#20141,1.);
#5669=VECTOR('',#20144,1.);
#5670=VECTOR('',#20147,1.);
#5671=VECTOR('',#20148,1.);
#5672=VECTOR('',#20151,1.);
#5673=VECTOR('',#20154,1.);
#5674=VECTOR('',#20155,1.);
#5675=VECTOR('',#20158,1.);
#5676=VECTOR('',#20161,1.);
#5677=VECTOR('',#20162,1.);
#5678=VECTOR('',#20165,1.);
#5679=VECTOR('',#20168,1.);
#5680=VECTOR('',#20169,1.);
#5681=VECTOR('',#20172,1.);
#5682=VECTOR('',#20175,1.);
#5683=VECTOR('',#20176,1.);
#5684=VECTOR('',#20179,1.);
#5685=VECTOR('',#20182,1.);
#5686=VECTOR('',#20183,1.);
#5687=VECTOR('',#20186,1.);
#5688=VECTOR('',#20189,1.);
#5689=VECTOR('',#20190,1.);
#5690=VECTOR('',#20193,1.);
#5691=VECTOR('',#20196,1.);
#5692=VECTOR('',#20197,1.);
#5693=VECTOR('',#20200,1.);
#5694=VECTOR('',#20203,1.);
#5695=VECTOR('',#20204,1.);
#5696=VECTOR('',#20207,1.);
#5697=VECTOR('',#20210,1.);
#5698=VECTOR('',#20211,1.);
#5699=VECTOR('',#20214,1.);
#5700=VECTOR('',#20217,1.);
#5701=VECTOR('',#20218,1.);
#5702=VECTOR('',#20221,1.);
#5703=VECTOR('',#20224,1.);
#5704=VECTOR('',#20225,1.);
#5705=VECTOR('',#20228,1.);
#5706=VECTOR('',#20231,1.);
#5707=VECTOR('',#20232,1.);
#5708=VECTOR('',#20235,1.);
#5709=VECTOR('',#20238,1.);
#5710=VECTOR('',#20239,1.);
#5711=VECTOR('',#20242,1.);
#5712=VECTOR('',#20245,1.);
#5713=VECTOR('',#20246,1.);
#5714=VECTOR('',#20249,1.);
#5715=VECTOR('',#20252,1.);
#5716=VECTOR('',#20253,1.);
#5717=VECTOR('',#20256,1.);
#5718=VECTOR('',#20259,1.);
#5719=VECTOR('',#20260,1.);
#5720=VECTOR('',#20263,1.);
#5721=VECTOR('',#20266,1.);
#5722=VECTOR('',#20267,1.);
#5723=VECTOR('',#20270,1.);
#5724=VECTOR('',#20273,1.);
#5725=VECTOR('',#20274,1.);
#5726=VECTOR('',#20277,1.);
#5727=VECTOR('',#20280,1.);
#5728=VECTOR('',#20281,1.);
#5729=VECTOR('',#20284,1.);
#5730=VECTOR('',#20287,1.);
#5731=VECTOR('',#20288,1.);
#5732=VECTOR('',#20291,1.);
#5733=VECTOR('',#20294,1.);
#5734=VECTOR('',#20295,1.);
#5735=VECTOR('',#20298,1.);
#5736=VECTOR('',#20301,1.);
#5737=VECTOR('',#20302,1.);
#5738=VECTOR('',#20305,1.);
#5739=VECTOR('',#20488,0.475);
#5740=VECTOR('',#20497,0.23);
#5741=VECTOR('',#20508,0.47);
#5742=VECTOR('',#20531,0.2);
#5743=VECTOR('',#20536,0.2);
#5744=VECTOR('',#20539,0.2);
#5745=VECTOR('',#20542,0.2);
#5746=VECTOR('',#20545,0.2);
#5747=VECTOR('',#20548,0.2);
#5748=VECTOR('',#20551,0.2);
#5749=VECTOR('',#20554,0.2);
#5750=VECTOR('',#20557,0.2);
#5751=VECTOR('',#20560,0.2);
#5752=VECTOR('',#20563,0.2);
#5753=VECTOR('',#20566,0.2);
#5754=VECTOR('',#20569,0.2);
#5755=VECTOR('',#20572,0.2);
#5756=VECTOR('',#20575,0.2);
#5757=VECTOR('',#20578,0.2);
#5758=VECTOR('',#20581,0.2);
#5759=VECTOR('',#20584,0.2);
#5760=VECTOR('',#20587,0.2);
#5761=VECTOR('',#20590,0.2);
#5762=VECTOR('',#20593,0.2);
#5763=VECTOR('',#20596,0.2);
#5764=VECTOR('',#20599,0.15555);
#5765=VECTOR('',#20604,0.15555);
#5766=VECTOR('',#20607,0.15555);
#5767=VECTOR('',#20610,0.15555);
#5768=VECTOR('',#20613,0.15555);
#5769=VECTOR('',#20616,0.15555);
#5770=VECTOR('',#20619,0.15555);
#5771=VECTOR('',#20622,0.15555);
#5772=VECTOR('',#20625,0.15555);
#5773=VECTOR('',#20628,0.15555);
#5774=VECTOR('',#20631,0.15555);
#5775=VECTOR('',#20634,0.15555);
#5776=VECTOR('',#20637,0.15555);
#5777=VECTOR('',#20640,0.15555);
#5778=VECTOR('',#20643,0.15555);
#5779=VECTOR('',#20646,0.15555);
#5780=VECTOR('',#20649,0.15555);
#5781=VECTOR('',#20652,0.15555);
#5782=VECTOR('',#20655,0.15555);
#5783=VECTOR('',#20658,0.15555);
#5784=VECTOR('',#20661,0.15555);
#5785=VECTOR('',#20664,0.15555);
#5786=VECTOR('',#20693,1.);
#5787=VECTOR('',#20694,1.);
#5788=VECTOR('',#20697,1.);
#5789=VECTOR('',#20698,1.);
#5790=VECTOR('',#20701,1.);
#5791=VECTOR('',#20702,1.);
#5792=VECTOR('',#20705,1.);
#5793=VECTOR('',#20706,1.);
#5794=VECTOR('',#20709,1.);
#5795=VECTOR('',#20710,1.);
#5796=VECTOR('',#20713,1.);
#5797=VECTOR('',#20714,1.);
#5798=VECTOR('',#20717,1.);
#5799=VECTOR('',#20718,1.);
#5800=VECTOR('',#20721,1.);
#5801=VECTOR('',#20722,1.);
#5802=VECTOR('',#20725,1.);
#5803=VECTOR('',#20726,1.);
#5804=VECTOR('',#20729,1.);
#5805=VECTOR('',#20730,1.);
#5806=VECTOR('',#20733,1.);
#5807=VECTOR('',#20734,1.);
#5808=VECTOR('',#20737,1.);
#5809=VECTOR('',#20738,1.);
#5810=VECTOR('',#20741,1.);
#5811=VECTOR('',#20742,1.);
#5812=VECTOR('',#20745,1.);
#5813=VECTOR('',#20746,1.);
#5814=VECTOR('',#20749,1.);
#5815=VECTOR('',#20750,1.);
#5816=VECTOR('',#20753,1.);
#5817=VECTOR('',#20754,1.);
#5818=VECTOR('',#20757,1.);
#5819=VECTOR('',#20758,1.);
#5820=VECTOR('',#20761,1.);
#5821=VECTOR('',#20762,1.);
#5822=VECTOR('',#20765,1.);
#5823=VECTOR('',#20766,1.);
#5824=VECTOR('',#20769,1.);
#5825=VECTOR('',#20770,1.);
#5826=VECTOR('',#20773,1.);
#5827=VECTOR('',#20774,1.);
#5828=VECTOR('',#20777,1.);
#5829=VECTOR('',#20778,1.);
#5830=VECTOR('',#20781,1.);
#5831=VECTOR('',#20782,1.);
#5832=VECTOR('',#20785,1.);
#5833=VECTOR('',#20786,1.);
#5834=VECTOR('',#20789,1.);
#5835=VECTOR('',#20790,1.);
#5836=VECTOR('',#20793,1.);
#5837=VECTOR('',#20794,1.);
#5838=VECTOR('',#20797,1.);
#5839=VECTOR('',#20798,1.);
#5840=VECTOR('',#20801,1.);
#5841=VECTOR('',#20802,1.);
#5842=VECTOR('',#20805,1.);
#5843=VECTOR('',#20806,1.);
#5844=VECTOR('',#20809,1.);
#5845=VECTOR('',#20810,1.);
#5846=VECTOR('',#20813,1.);
#5847=VECTOR('',#20814,1.);
#5848=VECTOR('',#20817,1.);
#5849=VECTOR('',#20818,1.);
#5850=VECTOR('',#20821,1.);
#5851=VECTOR('',#20822,1.);
#5852=VECTOR('',#20825,1.);
#5853=VECTOR('',#20826,1.);
#5854=VECTOR('',#20829,1.);
#5855=VECTOR('',#20830,1.);
#5856=VECTOR('',#20833,1.);
#5857=VECTOR('',#20834,1.);
#5858=VECTOR('',#20839,1.);
#5859=VECTOR('',#20844,1.);
#5860=VECTOR('',#20849,1.);
#5861=VECTOR('',#20854,1.);
#5862=VECTOR('',#20859,1.);
#5863=VECTOR('',#20864,1.);
#5864=VECTOR('',#20869,0.0866025403784439);
#5865=VECTOR('',#20886,1.);
#5866=VECTOR('',#20887,1.);
#5867=VECTOR('',#20888,1.);
#5868=VECTOR('',#20891,1.);
#5869=VECTOR('',#20892,1.);
#5870=VECTOR('',#20895,1.);
#5871=VECTOR('',#20896,1.);
#5872=VECTOR('',#20899,1.);
#5873=VECTOR('',#20900,1.);
#5874=VECTOR('',#20903,1.);
#5875=VECTOR('',#20904,1.);
#5876=VECTOR('',#20907,1.);
#5877=VECTOR('',#20908,1.);
#5878=VECTOR('',#20911,1.);
#5879=VECTOR('',#20912,1.);
#5880=VECTOR('',#20915,1.);
#5881=VECTOR('',#20916,1.);
#5882=VECTOR('',#20919,1.);
#5883=VECTOR('',#20920,1.);
#5884=VECTOR('',#20923,1.);
#5885=VECTOR('',#20926,1.);
#5886=VECTOR('',#20931,1.);
#5887=VECTOR('',#20934,1.);
#5888=VECTOR('',#20935,1.);
#5889=VECTOR('',#20938,1.);
#5890=VECTOR('',#20941,1.);
#5891=VECTOR('',#20944,1.);
#5892=VECTOR('',#20945,1.);
#5893=VECTOR('',#20948,1.);
#5894=VECTOR('',#20955,1.);
#5895=VECTOR('',#20964,1.);
#5896=VECTOR('',#20965,1.);
#5897=VECTOR('',#20968,1.);
#5898=VECTOR('',#20971,1.);
#5899=VECTOR('',#20972,1.);
#5900=VECTOR('',#20975,1.);
#5901=VECTOR('',#20978,1.);
#5902=VECTOR('',#20979,1.);
#5903=VECTOR('',#20982,1.);
#5904=VECTOR('',#20985,1.);
#5905=VECTOR('',#20986,1.);
#5906=VECTOR('',#20989,1.);
#5907=VECTOR('',#20992,1.);
#5908=VECTOR('',#20993,1.);
#5909=VECTOR('',#20996,1.);
#5910=VECTOR('',#20999,1.);
#5911=VECTOR('',#21000,1.);
#5912=VECTOR('',#21003,1.);
#5913=VECTOR('',#21006,1.);
#5914=VECTOR('',#21007,1.);
#5915=VECTOR('',#21010,1.);
#5916=VECTOR('',#21013,1.);
#5917=VECTOR('',#21014,1.);
#5918=VECTOR('',#21017,1.);
#5919=VECTOR('',#21020,1.);
#5920=VECTOR('',#21021,1.);
#5921=VECTOR('',#21024,1.);
#5922=VECTOR('',#21027,1.);
#5923=VECTOR('',#21028,1.);
#5924=VECTOR('',#21031,1.);
#5925=VECTOR('',#21034,1.);
#5926=VECTOR('',#21035,1.);
#5927=VECTOR('',#21038,1.);
#5928=VECTOR('',#21041,1.);
#5929=VECTOR('',#21042,1.);
#5930=VECTOR('',#21045,1.);
#5931=VECTOR('',#21048,1.);
#5932=VECTOR('',#21049,1.);
#5933=VECTOR('',#21052,1.);
#5934=VECTOR('',#21055,1.);
#5935=VECTOR('',#21056,1.);
#5936=VECTOR('',#21059,1.);
#5937=VECTOR('',#21062,1.);
#5938=VECTOR('',#21063,1.);
#5939=VECTOR('',#21066,1.);
#5940=VECTOR('',#21069,1.);
#5941=VECTOR('',#21070,1.);
#5942=VECTOR('',#21073,1.);
#5943=VECTOR('',#21076,1.);
#5944=VECTOR('',#21077,1.);
#5945=VECTOR('',#21080,1.);
#5946=VECTOR('',#21083,1.);
#5947=VECTOR('',#21084,1.);
#5948=VECTOR('',#21087,1.);
#5949=VECTOR('',#21090,1.);
#5950=VECTOR('',#21091,1.);
#5951=VECTOR('',#21094,1.);
#5952=VECTOR('',#21097,1.);
#5953=VECTOR('',#21098,1.);
#5954=VECTOR('',#21101,1.);
#5955=VECTOR('',#21104,1.);
#5956=VECTOR('',#21105,1.);
#5957=VECTOR('',#21108,1.);
#5958=VECTOR('',#21111,1.);
#5959=VECTOR('',#21112,1.);
#5960=VECTOR('',#21115,1.);
#5961=VECTOR('',#21118,1.);
#5962=VECTOR('',#21119,1.);
#5963=VECTOR('',#21122,1.);
#5964=VECTOR('',#21125,1.);
#5965=VECTOR('',#21126,1.);
#5966=VECTOR('',#21129,1.);
#5967=VECTOR('',#21132,1.);
#5968=VECTOR('',#21133,1.);
#5969=VECTOR('',#21136,1.);
#5970=VECTOR('',#21139,1.);
#5971=VECTOR('',#21140,1.);
#5972=VECTOR('',#21143,1.);
#5973=VECTOR('',#21146,1.);
#5974=VECTOR('',#21147,1.);
#5975=VECTOR('',#21150,1.);
#5976=VECTOR('',#21153,1.);
#5977=VECTOR('',#21154,1.);
#5978=VECTOR('',#21157,1.);
#5979=VECTOR('',#21160,1.);
#5980=VECTOR('',#21161,1.);
#5981=VECTOR('',#21164,1.);
#5982=VECTOR('',#21167,1.);
#5983=VECTOR('',#21168,1.);
#5984=VECTOR('',#21171,1.);
#5985=VECTOR('',#21174,1.);
#5986=VECTOR('',#21175,1.);
#5987=VECTOR('',#21178,1.);
#5988=VECTOR('',#21181,1.);
#5989=VECTOR('',#21182,1.);
#5990=VECTOR('',#21185,1.);
#5991=VECTOR('',#21188,1.);
#5992=VECTOR('',#21189,1.);
#5993=VECTOR('',#21192,1.);
#5994=VECTOR('',#21195,1.);
#5995=VECTOR('',#21196,1.);
#5996=VECTOR('',#21199,1.);
#5997=VECTOR('',#21202,1.);
#5998=VECTOR('',#21203,1.);
#5999=VECTOR('',#21206,1.);
#6000=VECTOR('',#21209,1.);
#6001=VECTOR('',#21210,1.);
#6002=VECTOR('',#21213,1.);
#6003=VECTOR('',#21364,0.18);
#6004=VECTOR('',#21369,0.33);
#6005=VECTOR('',#21376,0.2);
#6006=VECTOR('',#21381,0.2);
#6007=VECTOR('',#21384,0.2);
#6008=VECTOR('',#21387,0.2);
#6009=VECTOR('',#21390,0.2);
#6010=VECTOR('',#21393,0.2);
#6011=VECTOR('',#21396,0.2);
#6012=VECTOR('',#21399,0.2);
#6013=VECTOR('',#21402,0.2);
#6014=VECTOR('',#21405,0.2);
#6015=VECTOR('',#21408,0.2);
#6016=VECTOR('',#21411,0.15555);
#6017=VECTOR('',#21416,0.15555);
#6018=VECTOR('',#21419,0.15555);
#6019=VECTOR('',#21422,0.15555);
#6020=VECTOR('',#21425,0.15555);
#6021=VECTOR('',#21428,0.15555);
#6022=VECTOR('',#21431,0.15555);
#6023=VECTOR('',#21434,0.15555);
#6024=VECTOR('',#21437,0.15555);
#6025=VECTOR('',#21440,0.15555);
#6026=VECTOR('',#21443,0.15555);
#6027=VECTOR('',#21456,1.);
#6028=VECTOR('',#21457,1.);
#6029=VECTOR('',#21460,1.);
#6030=VECTOR('',#21463,1.);
#6031=VECTOR('',#21464,1.);
#6032=VECTOR('',#21467,1.);
#6033=VECTOR('',#21470,1.);
#6034=VECTOR('',#21471,1.);
#6035=VECTOR('',#21474,1.);
#6036=VECTOR('',#21477,1.);
#6037=VECTOR('',#21478,1.);
#6038=VECTOR('',#21481,1.);
#6039=VECTOR('',#21484,1.);
#6040=VECTOR('',#21485,1.);
#6041=VECTOR('',#21488,1.);
#6042=VECTOR('',#21491,1.);
#6043=VECTOR('',#21492,1.);
#6044=VECTOR('',#21495,1.);
#6045=VECTOR('',#21498,1.);
#6046=VECTOR('',#21499,1.);
#6047=VECTOR('',#21502,1.);
#6048=VECTOR('',#21505,1.);
#6049=VECTOR('',#21506,1.);
#6050=VECTOR('',#21509,1.);
#6051=VECTOR('',#21512,1.);
#6052=VECTOR('',#21513,1.);
#6053=VECTOR('',#21516,1.);
#6054=VECTOR('',#21519,1.);
#6055=VECTOR('',#21520,1.);
#6056=VECTOR('',#21523,1.);
#6057=VECTOR('',#21526,1.);
#6058=VECTOR('',#21527,1.);
#6059=VECTOR('',#21530,1.);
#6060=VECTOR('',#21533,1.);
#6061=VECTOR('',#21534,1.);
#6062=VECTOR('',#21537,1.);
#6063=VECTOR('',#21540,1.);
#6064=VECTOR('',#21541,1.);
#6065=VECTOR('',#21544,1.);
#6066=VECTOR('',#21547,1.);
#6067=VECTOR('',#21548,1.);
#6068=VECTOR('',#21551,1.);
#6069=VECTOR('',#21554,1.);
#6070=VECTOR('',#21555,1.);
#6071=VECTOR('',#21558,1.);
#6072=VECTOR('',#21561,1.);
#6073=VECTOR('',#21562,1.);
#6074=VECTOR('',#21565,1.);
#6075=VECTOR('',#21568,1.);
#6076=VECTOR('',#21569,1.);
#6077=VECTOR('',#21572,1.);
#6078=VECTOR('',#21575,1.);
#6079=VECTOR('',#21576,1.);
#6080=VECTOR('',#21579,1.);
#6081=VECTOR('',#21582,1.);
#6082=VECTOR('',#21583,1.);
#6083=VECTOR('',#21586,1.);
#6084=VECTOR('',#21589,1.);
#6085=VECTOR('',#21590,1.);
#6086=VECTOR('',#21593,1.);
#6087=VECTOR('',#21596,1.);
#6088=VECTOR('',#21597,1.);
#6089=VECTOR('',#21600,1.);
#6090=VECTOR('',#21603,1.);
#6091=VECTOR('',#21604,1.);
#6092=VECTOR('',#21607,1.);
#6093=VECTOR('',#21610,1.);
#6094=VECTOR('',#21611,1.);
#6095=VECTOR('',#21614,1.);
#6096=VECTOR('',#21617,1.);
#6097=VECTOR('',#21618,1.);
#6098=VECTOR('',#21621,1.);
#6099=VECTOR('',#21768,0.38);
#6100=VECTOR('',#21777,0.185);
#6101=VECTOR('',#21788,0.375);
#6102=VERTEX_POINT('',#21836);
#6103=VERTEX_POINT('',#21837);
#6104=VERTEX_POINT('',#21839);
#6105=VERTEX_POINT('',#21841);
#6106=VERTEX_POINT('',#21843);
#6107=VERTEX_POINT('',#21845);
#6108=VERTEX_POINT('',#21849);
#6109=VERTEX_POINT('',#21851);
#6110=VERTEX_POINT('',#21853);
#6111=VERTEX_POINT('',#21857);
#6112=VERTEX_POINT('',#21859);
#6113=VERTEX_POINT('',#21861);
#6114=VERTEX_POINT('',#21865);
#6115=VERTEX_POINT('',#21869);
#6116=VERTEX_POINT('',#21871);
#6117=VERTEX_POINT('',#21873);
#6118=VERTEX_POINT('',#21877);
#6119=VERTEX_POINT('',#21879);
#6120=VERTEX_POINT('',#21883);
#6121=VERTEX_POINT('',#21884);
#6122=VERTEX_POINT('',#21886);
#6123=VERTEX_POINT('',#21888);
#6124=VERTEX_POINT('',#21890);
#6125=VERTEX_POINT('',#21892);
#6126=VERTEX_POINT('',#21896);
#6127=VERTEX_POINT('',#21898);
#6128=VERTEX_POINT('',#21902);
#6129=VERTEX_POINT('',#21904);
#6130=VERTEX_POINT('',#21908);
#6131=VERTEX_POINT('',#21910);
#6132=VERTEX_POINT('',#21914);
#6133=VERTEX_POINT('',#21915);
#6134=VERTEX_POINT('',#21917);
#6135=VERTEX_POINT('',#21919);
#6136=VERTEX_POINT('',#21921);
#6137=VERTEX_POINT('',#21923);
#6138=VERTEX_POINT('',#21927);
#6139=VERTEX_POINT('',#21929);
#6140=VERTEX_POINT('',#21931);
#6141=VERTEX_POINT('',#21935);
#6142=VERTEX_POINT('',#21939);
#6143=VERTEX_POINT('',#21941);
#6144=VERTEX_POINT('',#21945);
#6145=VERTEX_POINT('',#21946);
#6146=VERTEX_POINT('',#21948);
#6147=VERTEX_POINT('',#21950);
#6148=VERTEX_POINT('',#21952);
#6149=VERTEX_POINT('',#21954);
#6150=VERTEX_POINT('',#21958);
#6151=VERTEX_POINT('',#21960);
#6152=VERTEX_POINT('',#21962);
#6153=VERTEX_POINT('',#21964);
#6154=VERTEX_POINT('',#21968);
#6155=VERTEX_POINT('',#21972);
#6156=VERTEX_POINT('',#21974);
#6157=VERTEX_POINT('',#21976);
#6158=VERTEX_POINT('',#21980);
#6159=VERTEX_POINT('',#21982);
#6160=VERTEX_POINT('',#21986);
#6161=VERTEX_POINT('',#21988);
#6162=VERTEX_POINT('',#21992);
#6163=VERTEX_POINT('',#21996);
#6164=VERTEX_POINT('',#21999);
#6165=VERTEX_POINT('',#22003);
#6166=VERTEX_POINT('',#22006);
#6167=VERTEX_POINT('',#22117);
#6168=VERTEX_POINT('',#22119);
#6169=VERTEX_POINT('',#22147);
#6170=VERTEX_POINT('',#22149);
#6171=VERTEX_POINT('',#22173);
#6172=VERTEX_POINT('',#22174);
#6173=VERTEX_POINT('',#22176);
#6174=VERTEX_POINT('',#22178);
#6175=VERTEX_POINT('',#22180);
#6176=VERTEX_POINT('',#22182);
#6177=VERTEX_POINT('',#22186);
#6178=VERTEX_POINT('',#22188);
#6179=VERTEX_POINT('',#22192);
#6180=VERTEX_POINT('',#22194);
#6181=VERTEX_POINT('',#22196);
#6182=VERTEX_POINT('',#22200);
#6183=VERTEX_POINT('',#22202);
#6184=VERTEX_POINT('',#22206);
#6185=VERTEX_POINT('',#22207);
#6186=VERTEX_POINT('',#22209);
#6187=VERTEX_POINT('',#22211);
#6188=VERTEX_POINT('',#22213);
#6189=VERTEX_POINT('',#22215);
#6190=VERTEX_POINT('',#22219);
#6191=VERTEX_POINT('',#22221);
#6192=VERTEX_POINT('',#22223);
#6193=VERTEX_POINT('',#22227);
#6194=VERTEX_POINT('',#22231);
#6195=VERTEX_POINT('',#22233);
#6196=VERTEX_POINT('',#22237);
#6197=VERTEX_POINT('',#22238);
#6198=VERTEX_POINT('',#22243);
#6199=VERTEX_POINT('',#22244);
#6200=VERTEX_POINT('',#22252);
#6201=VERTEX_POINT('',#22254);
#6202=VERTEX_POINT('',#22256);
#6203=VERTEX_POINT('',#22260);
#6204=VERTEX_POINT('',#22264);
#6205=VERTEX_POINT('',#22268);
#6206=VERTEX_POINT('',#22272);
#6207=VERTEX_POINT('',#22278);
#6208=VERTEX_POINT('',#22280);
#6209=VERTEX_POINT('',#22282);
#6210=VERTEX_POINT('',#22286);
#6211=VERTEX_POINT('',#22287);
#6212=VERTEX_POINT('',#22292);
#6213=VERTEX_POINT('',#22293);
#6214=VERTEX_POINT('',#22298);
#6215=VERTEX_POINT('',#22299);
#6216=VERTEX_POINT('',#22304);
#6217=VERTEX_POINT('',#22318);
#6218=VERTEX_POINT('',#22322);
#6219=VERTEX_POINT('',#22327);
#6220=VERTEX_POINT('',#22331);
#6221=VERTEX_POINT('',#22335);
#6222=VERTEX_POINT('',#22339);
#6223=VERTEX_POINT('',#22344);
#6224=VERTEX_POINT('',#22348);
#6225=VERTEX_POINT('',#22352);
#6226=VERTEX_POINT('',#22353);
#6227=VERTEX_POINT('',#22358);
#6228=VERTEX_POINT('',#22359);
#6229=VERTEX_POINT('',#22364);
#6230=VERTEX_POINT('',#22369);
#6231=VERTEX_POINT('',#22373);
#6232=VERTEX_POINT('',#22375);
#6233=VERTEX_POINT('',#22379);
#6234=VERTEX_POINT('',#22380);
#6235=VERTEX_POINT('',#22386);
#6236=VERTEX_POINT('',#22390);
#6237=VERTEX_POINT('',#22394);
#6238=VERTEX_POINT('',#22396);
#6239=VERTEX_POINT('',#22400);
#6240=VERTEX_POINT('',#22407);
#6241=VERTEX_POINT('',#22481);
#6242=VERTEX_POINT('',#22502);
#6243=VERTEX_POINT('',#22504);
#6244=VERTEX_POINT('',#22506);
#6245=VERTEX_POINT('',#22510);
#6246=VERTEX_POINT('',#22519);
#6247=VERTEX_POINT('',#22521);
#6248=VERTEX_POINT('',#22525);
#6249=VERTEX_POINT('',#22527);
#6250=VERTEX_POINT('',#22531);
#6251=VERTEX_POINT('',#22532);
#6252=VERTEX_POINT('',#22537);
#6253=VERTEX_POINT('',#22538);
#6254=VERTEX_POINT('',#22543);
#6255=VERTEX_POINT('',#22548);
#6256=VERTEX_POINT('',#22552);
#6257=VERTEX_POINT('',#22554);
#6258=VERTEX_POINT('',#22558);
#6259=VERTEX_POINT('',#22559);
#6260=VERTEX_POINT('',#22567);
#6261=VERTEX_POINT('',#22569);
#6262=VERTEX_POINT('',#22573);
#6263=VERTEX_POINT('',#22574);
#6264=VERTEX_POINT('',#22582);
#6265=VERTEX_POINT('',#22584);
#6266=VERTEX_POINT('',#22588);
#6267=VERTEX_POINT('',#22595);
#6268=VERTEX_POINT('',#22599);
#6269=VERTEX_POINT('',#22600);
#6270=VERTEX_POINT('',#22608);
#6271=VERTEX_POINT('',#22612);
#6272=VERTEX_POINT('',#22618);
#6273=VERTEX_POINT('',#22624);
#6274=VERTEX_POINT('',#22628);
#6275=VERTEX_POINT('',#22635);
#6276=VERTEX_POINT('',#22639);
#6277=VERTEX_POINT('',#22671);
#6278=VERTEX_POINT('',#22673);
#6279=VERTEX_POINT('',#22676);
#6280=VERTEX_POINT('',#22680);
#6281=VERTEX_POINT('',#22681);
#6282=VERTEX_POINT('',#22692);
#6283=VERTEX_POINT('',#22694);
#6284=VERTEX_POINT('',#22706);
#6285=VERTEX_POINT('',#22717);
#6286=VERTEX_POINT('',#22730);
#6287=VERTEX_POINT('',#22732);
#6288=VERTEX_POINT('',#22736);
#6289=VERTEX_POINT('',#22739);
#6290=VERTEX_POINT('',#22740);
#6291=VERTEX_POINT('',#22783);
#6292=VERTEX_POINT('',#22785);
#6293=VERTEX_POINT('',#22796);
#6294=VERTEX_POINT('',#22826);
#6295=VERTEX_POINT('',#22827);
#6296=VERTEX_POINT('',#22831);
#6297=VERTEX_POINT('',#22833);
#6298=VERTEX_POINT('',#22844);
#6299=VERTEX_POINT('',#22877);
#6300=VERTEX_POINT('',#22880);
#6301=VERTEX_POINT('',#22884);
#6302=VERTEX_POINT('',#22888);
#6303=VERTEX_POINT('',#22891);
#6304=VERTEX_POINT('',#22895);
#6305=VERTEX_POINT('',#22900);
#6306=VERTEX_POINT('',#22904);
#6307=VERTEX_POINT('',#22907);
#6308=VERTEX_POINT('',#22912);
#6309=VERTEX_POINT('',#22918);
#6310=VERTEX_POINT('',#22920);
#6311=VERTEX_POINT('',#22922);
#6312=VERTEX_POINT('',#22926);
#6313=VERTEX_POINT('',#22928);
#6314=VERTEX_POINT('',#22933);
#6315=VERTEX_POINT('',#22935);
#6316=VERTEX_POINT('',#22939);
#6317=VERTEX_POINT('',#22941);
#6318=VERTEX_POINT('',#22945);
#6319=VERTEX_POINT('',#22947);
#6320=VERTEX_POINT('',#22951);
#6321=VERTEX_POINT('',#22953);
#6322=VERTEX_POINT('',#22957);
#6323=VERTEX_POINT('',#22963);
#6324=VERTEX_POINT('',#22964);
#6325=VERTEX_POINT('',#22966);
#6326=VERTEX_POINT('',#22968);
#6327=VERTEX_POINT('',#22970);
#6328=VERTEX_POINT('',#22972);
#6329=VERTEX_POINT('',#22976);
#6330=VERTEX_POINT('',#22978);
#6331=VERTEX_POINT('',#22980);
#6332=VERTEX_POINT('',#22982);
#6333=VERTEX_POINT('',#22986);
#6334=VERTEX_POINT('',#22988);
#6335=VERTEX_POINT('',#22990);
#6336=VERTEX_POINT('',#22992);
#6337=VERTEX_POINT('',#22994);
#6338=VERTEX_POINT('',#22996);
#6339=VERTEX_POINT('',#23000);
#6340=VERTEX_POINT('',#23004);
#6341=VERTEX_POINT('',#23006);
#6342=VERTEX_POINT('',#23008);
#6343=VERTEX_POINT('',#23010);
#6344=VERTEX_POINT('',#23016);
#6345=VERTEX_POINT('',#23018);
#6346=VERTEX_POINT('',#23020);
#6347=VERTEX_POINT('',#23022);
#6348=VERTEX_POINT('',#23024);
#6349=VERTEX_POINT('',#23028);
#6350=VERTEX_POINT('',#23030);
#6351=VERTEX_POINT('',#23034);
#6352=VERTEX_POINT('',#23036);
#6353=VERTEX_POINT('',#23038);
#6354=VERTEX_POINT('',#23040);
#6355=VERTEX_POINT('',#23042);
#6356=VERTEX_POINT('',#23046);
#6357=VERTEX_POINT('',#23047);
#6358=VERTEX_POINT('',#23050);
#6359=VERTEX_POINT('',#23052);
#6360=VERTEX_POINT('',#23056);
#6361=VERTEX_POINT('',#23058);
#6362=VERTEX_POINT('',#23060);
#6363=VERTEX_POINT('',#23062);
#6364=VERTEX_POINT('',#23066);
#6365=VERTEX_POINT('',#23070);
#6366=VERTEX_POINT('',#23072);
#6367=VERTEX_POINT('',#23076);
#6368=VERTEX_POINT('',#23080);
#6369=VERTEX_POINT('',#23082);
#6370=VERTEX_POINT('',#23084);
#6371=VERTEX_POINT('',#23086);
#6372=VERTEX_POINT('',#23088);
#6373=VERTEX_POINT('',#23092);
#6374=VERTEX_POINT('',#23093);
#6375=VERTEX_POINT('',#23096);
#6376=VERTEX_POINT('',#23098);
#6377=VERTEX_POINT('',#23102);
#6378=VERTEX_POINT('',#23104);
#6379=VERTEX_POINT('',#23106);
#6380=VERTEX_POINT('',#23108);
#6381=VERTEX_POINT('',#23112);
#6382=VERTEX_POINT('',#23116);
#6383=VERTEX_POINT('',#23118);
#6384=VERTEX_POINT('',#23122);
#6385=VERTEX_POINT('',#23124);
#6386=VERTEX_POINT('',#23128);
#6387=VERTEX_POINT('',#23130);
#6388=VERTEX_POINT('',#23132);
#6389=VERTEX_POINT('',#23137);
#6390=VERTEX_POINT('',#23139);
#6391=VERTEX_POINT('',#23141);
#6392=VERTEX_POINT('',#23143);
#6393=VERTEX_POINT('',#23145);
#6394=VERTEX_POINT('',#23147);
#6395=VERTEX_POINT('',#23151);
#6396=VERTEX_POINT('',#23155);
#6397=VERTEX_POINT('',#23157);
#6398=VERTEX_POINT('',#23159);
#6399=VERTEX_POINT('',#23161);
#6400=VERTEX_POINT('',#23166);
#6401=VERTEX_POINT('',#23168);
#6402=VERTEX_POINT('',#23172);
#6403=VERTEX_POINT('',#23178);
#6404=VERTEX_POINT('',#23188);
#6405=VERTEX_POINT('',#23190);
#6406=VERTEX_POINT('',#23194);
#6407=VERTEX_POINT('',#23199);
#6408=VERTEX_POINT('',#23204);
#6409=VERTEX_POINT('',#23206);
#6410=VERTEX_POINT('',#23208);
#6411=VERTEX_POINT('',#23210);
#6412=VERTEX_POINT('',#23212);
#6413=VERTEX_POINT('',#23214);
#6414=VERTEX_POINT('',#23220);
#6415=VERTEX_POINT('',#23224);
#6416=VERTEX_POINT('',#23228);
#6417=VERTEX_POINT('',#23233);
#6418=VERTEX_POINT('',#23234);
#6419=VERTEX_POINT('',#23237);
#6420=VERTEX_POINT('',#23239);
#6421=VERTEX_POINT('',#23243);
#6422=VERTEX_POINT('',#23244);
#6423=VERTEX_POINT('',#23249);
#6424=VERTEX_POINT('',#23253);
#6425=VERTEX_POINT('',#23257);
#6426=VERTEX_POINT('',#23260);
#6427=VERTEX_POINT('',#23262);
#6428=VERTEX_POINT('',#23264);
#6429=VERTEX_POINT('',#23268);
#6430=VERTEX_POINT('',#23273);
#6431=VERTEX_POINT('',#23279);
#6432=VERTEX_POINT('',#23283);
#6433=VERTEX_POINT('',#23284);
#6434=VERTEX_POINT('',#23289);
#6435=VERTEX_POINT('',#23293);
#6436=VERTEX_POINT('',#23296);
#6437=VERTEX_POINT('',#23300);
#6438=VERTEX_POINT('',#23301);
#6439=VERTEX_POINT('',#23306);
#6440=VERTEX_POINT('',#23310);
#6441=VERTEX_POINT('',#23313);
#6442=VERTEX_POINT('',#23317);
#6443=VERTEX_POINT('',#23321);
#6444=VERTEX_POINT('',#23325);
#6445=VERTEX_POINT('',#23329);
#6446=VERTEX_POINT('',#23333);
#6447=VERTEX_POINT('',#23337);
#6448=VERTEX_POINT('',#23339);
#6449=VERTEX_POINT('',#23343);
#6450=VERTEX_POINT('',#23344);
#6451=VERTEX_POINT('',#23346);
#6452=VERTEX_POINT('',#23348);
#6453=VERTEX_POINT('',#23351);
#6454=VERTEX_POINT('',#23353);
#6455=VERTEX_POINT('',#23355);
#6456=VERTEX_POINT('',#23357);
#6457=VERTEX_POINT('',#23359);
#6458=VERTEX_POINT('',#23364);
#6459=VERTEX_POINT('',#23390);
#6460=VERTEX_POINT('',#23393);
#6461=VERTEX_POINT('',#23397);
#6462=VERTEX_POINT('',#23401);
#6463=VERTEX_POINT('',#23407);
#6464=VERTEX_POINT('',#23408);
#6465=VERTEX_POINT('',#23410);
#6466=VERTEX_POINT('',#23454);
#6467=VERTEX_POINT('',#23500);
#6468=VERTEX_POINT('',#23501);
#6469=VERTEX_POINT('',#23590);
#6470=VERTEX_POINT('',#23591);
#6471=VERTEX_POINT('',#23593);
#6472=VERTEX_POINT('',#23608);
#6473=VERTEX_POINT('',#23622);
#6474=VERTEX_POINT('',#23623);
#6475=VERTEX_POINT('',#23625);
#6476=VERTEX_POINT('',#23809);
#6477=VERTEX_POINT('',#23810);
#6478=VERTEX_POINT('',#23817);
#6479=VERTEX_POINT('',#23825);
#6480=VERTEX_POINT('',#23843);
#6481=VERTEX_POINT('',#23939);
#6482=VERTEX_POINT('',#23946);
#6483=VERTEX_POINT('',#23991);
#6484=VERTEX_POINT('',#23992);
#6485=VERTEX_POINT('',#23994);
#6486=VERTEX_POINT('',#24040);
#6487=VERTEX_POINT('',#24042);
#6488=VERTEX_POINT('',#24044);
#6489=VERTEX_POINT('',#24046);
#6490=VERTEX_POINT('',#24083);
#6491=VERTEX_POINT('',#24084);
#6492=VERTEX_POINT('',#24086);
#6493=VERTEX_POINT('',#24246);
#6494=VERTEX_POINT('',#24253);
#6495=VERTEX_POINT('',#24383);
#6496=VERTEX_POINT('',#24388);
#6497=VERTEX_POINT('',#24402);
#6498=VERTEX_POINT('',#24438);
#6499=VERTEX_POINT('',#24450);
#6500=VERTEX_POINT('',#24456);
#6501=VERTEX_POINT('',#24479);
#6502=VERTEX_POINT('',#24494);
#6503=VERTEX_POINT('',#24498);
#6504=VERTEX_POINT('',#24500);
#6505=VERTEX_POINT('',#24504);
#6506=VERTEX_POINT('',#24508);
#6507=VERTEX_POINT('',#24510);
#6508=VERTEX_POINT('',#24512);
#6509=VERTEX_POINT('',#24516);
#6510=VERTEX_POINT('',#24527);
#6511=VERTEX_POINT('',#24529);
#6512=VERTEX_POINT('',#24533);
#6513=VERTEX_POINT('',#24537);
#6514=VERTEX_POINT('',#24539);
#6515=VERTEX_POINT('',#24545);
#6516=VERTEX_POINT('',#24549);
#6517=VERTEX_POINT('',#24551);
#6518=VERTEX_POINT('',#24555);
#6519=VERTEX_POINT('',#24561);
#6520=VERTEX_POINT('',#24577);
#6521=VERTEX_POINT('',#24583);
#6522=VERTEX_POINT('',#24584);
#6523=VERTEX_POINT('',#24586);
#6524=VERTEX_POINT('',#24597);
#6525=VERTEX_POINT('',#24607);
#6526=VERTEX_POINT('',#24608);
#6527=VERTEX_POINT('',#24655);
#6528=VERTEX_POINT('',#24656);
#6529=VERTEX_POINT('',#24703);
#6530=VERTEX_POINT('',#24704);
#6531=VERTEX_POINT('',#24757);
#6532=VERTEX_POINT('',#24758);
#6533=VERTEX_POINT('',#24805);
#6534=VERTEX_POINT('',#24806);
#6535=VERTEX_POINT('',#24853);
#6536=VERTEX_POINT('',#24854);
#6537=VERTEX_POINT('',#24856);
#6538=VERTEX_POINT('',#24864);
#6539=VERTEX_POINT('',#24872);
#6540=VERTEX_POINT('',#24873);
#6541=VERTEX_POINT('',#24897);
#6542=VERTEX_POINT('',#24898);
#6543=VERTEX_POINT('',#24921);
#6544=VERTEX_POINT('',#24922);
#6545=VERTEX_POINT('',#24946);
#6546=VERTEX_POINT('',#24947);
#6547=VERTEX_POINT('',#24971);
#6548=VERTEX_POINT('',#24972);
#6549=VERTEX_POINT('',#24995);
#6550=VERTEX_POINT('',#25048);
#6551=VERTEX_POINT('',#25050);
#6552=VERTEX_POINT('',#25305);
#6553=VERTEX_POINT('',#25368);
#6554=VERTEX_POINT('',#25371);
#6555=VERTEX_POINT('',#25633);
#6556=VERTEX_POINT('',#25634);
#6557=VERTEX_POINT('',#25638);
#6558=VERTEX_POINT('',#25642);
#6559=VERTEX_POINT('',#25646);
#6560=VERTEX_POINT('',#25650);
#6561=VERTEX_POINT('',#25657);
#6562=VERTEX_POINT('',#25658);
#6563=VERTEX_POINT('',#25660);
#6564=VERTEX_POINT('',#25665);
#6565=VERTEX_POINT('',#25669);
#6566=VERTEX_POINT('',#25674);
#6567=VERTEX_POINT('',#25678);
#6568=VERTEX_POINT('',#25683);
#6569=VERTEX_POINT('',#25687);
#6570=VERTEX_POINT('',#25692);
#6571=VERTEX_POINT('',#25696);
#6572=VERTEX_POINT('',#25701);
#6573=VERTEX_POINT('',#25705);
#6574=VERTEX_POINT('',#25710);
#6575=VERTEX_POINT('',#25716);
#6576=VERTEX_POINT('',#25718);
#6577=VERTEX_POINT('',#25722);
#6578=VERTEX_POINT('',#25726);
#6579=VERTEX_POINT('',#25730);
#6580=VERTEX_POINT('',#25734);
#6581=VERTEX_POINT('',#25738);
#6582=VERTEX_POINT('',#25742);
#6583=VERTEX_POINT('',#25746);
#6584=VERTEX_POINT('',#25750);
#6585=VERTEX_POINT('',#25761);
#6586=VERTEX_POINT('',#25769);
#6587=VERTEX_POINT('',#25782);
#6588=VERTEX_POINT('',#25789);
#6589=VERTEX_POINT('',#25795);
#6590=VERTEX_POINT('',#25796);
#6591=VERTEX_POINT('',#25798);
#6592=VERTEX_POINT('',#25809);
#6593=VERTEX_POINT('',#25819);
#6594=VERTEX_POINT('',#25820);
#6595=VERTEX_POINT('',#25867);
#6596=VERTEX_POINT('',#25868);
#6597=VERTEX_POINT('',#25915);
#6598=VERTEX_POINT('',#25916);
#6599=VERTEX_POINT('',#25969);
#6600=VERTEX_POINT('',#25970);
#6601=VERTEX_POINT('',#26017);
#6602=VERTEX_POINT('',#26018);
#6603=VERTEX_POINT('',#26020);
#6604=VERTEX_POINT('',#26027);
#6605=VERTEX_POINT('',#26028);
#6606=VERTEX_POINT('',#26040);
#6607=VERTEX_POINT('',#26052);
#6608=VERTEX_POINT('',#26053);
#6609=VERTEX_POINT('',#26077);
#6610=VERTEX_POINT('',#26078);
#6611=VERTEX_POINT('',#26102);
#6612=VERTEX_POINT('',#26103);
#6613=VERTEX_POINT('',#26126);
#6614=VERTEX_POINT('',#26179);
#6615=VERTEX_POINT('',#26181);
#6616=VERTEX_POINT('',#26391);
#6617=VERTEX_POINT('',#26454);
#6618=VERTEX_POINT('',#26457);
#6619=VERTEX_POINT('',#26674);
#6620=VERTEX_POINT('',#26675);
#6621=VERTEX_POINT('',#26679);
#6622=VERTEX_POINT('',#26683);
#6623=VERTEX_POINT('',#26687);
#6624=VERTEX_POINT('',#26691);
#6625=VERTEX_POINT('',#26698);
#6626=VERTEX_POINT('',#26699);
#6627=VERTEX_POINT('',#26701);
#6628=VERTEX_POINT('',#26706);
#6629=VERTEX_POINT('',#26710);
#6630=VERTEX_POINT('',#26715);
#6631=VERTEX_POINT('',#26719);
#6632=VERTEX_POINT('',#26724);
#6633=VERTEX_POINT('',#26728);
#6634=VERTEX_POINT('',#26733);
#6635=VERTEX_POINT('',#26737);
#6636=VERTEX_POINT('',#26742);
#6637=VERTEX_POINT('',#26746);
#6638=VERTEX_POINT('',#26751);
#6639=VERTEX_POINT('',#26757);
#6640=VERTEX_POINT('',#26759);
#6641=VERTEX_POINT('',#26763);
#6642=VERTEX_POINT('',#26767);
#6643=VERTEX_POINT('',#26771);
#6644=VERTEX_POINT('',#26775);
#6645=VERTEX_POINT('',#26779);
#6646=VERTEX_POINT('',#26783);
#6647=VERTEX_POINT('',#26787);
#6648=VERTEX_POINT('',#26791);
#6649=VERTEX_POINT('',#26802);
#6650=VERTEX_POINT('',#26810);
#6651=VERTEX_POINT('',#26823);
#6652=VERTEX_POINT('',#26830);
#6653=VERTEX_POINT('',#26836);
#6654=VERTEX_POINT('',#26837);
#6655=VERTEX_POINT('',#26839);
#6656=VERTEX_POINT('',#26841);
#6657=VERTEX_POINT('',#26843);
#6658=VERTEX_POINT('',#26845);
#6659=VERTEX_POINT('',#26849);
#6660=VERTEX_POINT('',#26851);
#6661=VERTEX_POINT('',#26853);
#6662=VERTEX_POINT('',#26857);
#6663=VERTEX_POINT('',#26859);
#6664=VERTEX_POINT('',#26863);
#6665=VERTEX_POINT('',#26865);
#6666=VERTEX_POINT('',#26869);
#6667=VERTEX_POINT('',#26870);
#6668=VERTEX_POINT('',#26872);
#6669=VERTEX_POINT('',#26874);
#6670=VERTEX_POINT('',#26878);
#6671=VERTEX_POINT('',#26880);
#6672=VERTEX_POINT('',#26884);
#6673=VERTEX_POINT('',#26886);
#6674=VERTEX_POINT('',#26890);
#6675=VERTEX_POINT('',#26892);
#6676=VERTEX_POINT('',#26894);
#6677=VERTEX_POINT('',#27017);
#6678=VERTEX_POINT('',#27018);
#6679=VERTEX_POINT('',#27020);
#6680=VERTEX_POINT('',#27086);
#6681=VERTEX_POINT('',#27089);
#6682=VERTEX_POINT('',#27091);
#6683=VERTEX_POINT('',#27095);
#6684=VERTEX_POINT('',#27096);
#6685=VERTEX_POINT('',#27129);
#6686=VERTEX_POINT('',#27133);
#6687=VERTEX_POINT('',#27139);
#6688=VERTEX_POINT('',#27143);
#6689=VERTEX_POINT('',#27250);
#6690=VERTEX_POINT('',#27252);
#6691=VERTEX_POINT('',#27263);
#6692=VERTEX_POINT('',#27289);
#6693=VERTEX_POINT('',#27291);
#6694=VERTEX_POINT('',#27295);
#6695=VERTEX_POINT('',#27299);
#6696=VERTEX_POINT('',#27302);
#6697=VERTEX_POINT('',#27303);
#6698=VERTEX_POINT('',#27305);
#6699=VERTEX_POINT('',#27307);
#6700=VERTEX_POINT('',#27311);
#6701=VERTEX_POINT('',#27312);
#6702=VERTEX_POINT('',#27323);
#6703=VERTEX_POINT('',#27325);
#6704=VERTEX_POINT('',#27330);
#6705=VERTEX_POINT('',#27331);
#6706=VERTEX_POINT('',#27333);
#6707=VERTEX_POINT('',#27335);
#6708=VERTEX_POINT('',#27337);
#6709=VERTEX_POINT('',#27339);
#6710=VERTEX_POINT('',#27343);
#6711=VERTEX_POINT('',#27345);
#6712=VERTEX_POINT('',#27347);
#6713=VERTEX_POINT('',#27349);
#6714=VERTEX_POINT('',#27353);
#6715=VERTEX_POINT('',#27355);
#6716=VERTEX_POINT('',#27357);
#6717=VERTEX_POINT('',#27361);
#6718=VERTEX_POINT('',#27365);
#6719=VERTEX_POINT('',#27367);
#6720=VERTEX_POINT('',#27372);
#6721=VERTEX_POINT('',#27374);
#6722=VERTEX_POINT('',#27376);
#6723=VERTEX_POINT('',#27381);
#6724=VERTEX_POINT('',#27387);
#6725=VERTEX_POINT('',#27388);
#6726=VERTEX_POINT('',#27390);
#6727=VERTEX_POINT('',#27395);
#6728=VERTEX_POINT('',#27399);
#6729=VERTEX_POINT('',#27401);
#6730=VERTEX_POINT('',#27403);
#6731=VERTEX_POINT('',#27405);
#6732=VERTEX_POINT('',#27407);
#6733=VERTEX_POINT('',#27411);
#6734=VERTEX_POINT('',#27413);
#6735=VERTEX_POINT('',#27415);
#6736=VERTEX_POINT('',#27419);
#6737=VERTEX_POINT('',#27426);
#6738=VERTEX_POINT('',#27428);
#6739=VERTEX_POINT('',#27432);
#6740=VERTEX_POINT('',#27433);
#6741=VERTEX_POINT('',#27435);
#6742=VERTEX_POINT('',#27437);
#6743=VERTEX_POINT('',#27441);
#6744=VERTEX_POINT('',#27442);
#6745=VERTEX_POINT('',#27444);
#6746=VERTEX_POINT('',#27446);
#6747=VERTEX_POINT('',#27450);
#6748=VERTEX_POINT('',#27451);
#6749=VERTEX_POINT('',#27458);
#6750=VERTEX_POINT('',#27460);
#6751=VERTEX_POINT('',#27464);
#6752=VERTEX_POINT('',#27468);
#6753=VERTEX_POINT('',#27474);
#6754=VERTEX_POINT('',#27476);
#6755=VERTEX_POINT('',#27478);
#6756=VERTEX_POINT('',#27480);
#6757=VERTEX_POINT('',#27483);
#6758=VERTEX_POINT('',#27487);
#6759=VERTEX_POINT('',#27490);
#6760=VERTEX_POINT('',#27494);
#6761=VERTEX_POINT('',#27498);
#6762=VERTEX_POINT('',#27502);
#6763=VERTEX_POINT('',#27513);
#6764=VERTEX_POINT('',#27517);
#6765=VERTEX_POINT('',#27521);
#6766=VERTEX_POINT('',#27525);
#6767=VERTEX_POINT('',#27526);
#6768=VERTEX_POINT('',#27528);
#6769=VERTEX_POINT('',#27530);
#6770=VERTEX_POINT('',#27533);
#6771=VERTEX_POINT('',#27535);
#6772=VERTEX_POINT('',#27553);
#6773=VERTEX_POINT('',#27557);
#6774=VERTEX_POINT('',#27561);
#6775=VERTEX_POINT('',#27565);
#6776=VERTEX_POINT('',#27586);
#6777=VERTEX_POINT('',#27587);
#6778=VERTEX_POINT('',#27589);
#6779=VERTEX_POINT('',#27600);
#6780=VERTEX_POINT('',#27610);
#6781=VERTEX_POINT('',#27611);
#6782=VERTEX_POINT('',#27658);
#6783=VERTEX_POINT('',#27659);
#6784=VERTEX_POINT('',#27706);
#6785=VERTEX_POINT('',#27707);
#6786=VERTEX_POINT('',#27760);
#6787=VERTEX_POINT('',#27761);
#6788=VERTEX_POINT('',#27808);
#6789=VERTEX_POINT('',#27809);
#6790=VERTEX_POINT('',#27856);
#6791=VERTEX_POINT('',#27857);
#6792=VERTEX_POINT('',#27904);
#6793=VERTEX_POINT('',#27905);
#6794=VERTEX_POINT('',#27955);
#6795=VERTEX_POINT('',#27956);
#6796=VERTEX_POINT('',#28003);
#6797=VERTEX_POINT('',#28004);
#6798=VERTEX_POINT('',#28051);
#6799=VERTEX_POINT('',#28052);
#6800=VERTEX_POINT('',#28105);
#6801=VERTEX_POINT('',#28106);
#6802=VERTEX_POINT('',#28153);
#6803=VERTEX_POINT('',#28154);
#6804=VERTEX_POINT('',#28201);
#6805=VERTEX_POINT('',#28202);
#6806=VERTEX_POINT('',#28255);
#6807=VERTEX_POINT('',#28256);
#6808=VERTEX_POINT('',#28303);
#6809=VERTEX_POINT('',#28304);
#6810=VERTEX_POINT('',#28351);
#6811=VERTEX_POINT('',#28352);
#6812=VERTEX_POINT('',#28405);
#6813=VERTEX_POINT('',#28406);
#6814=VERTEX_POINT('',#28453);
#6815=VERTEX_POINT('',#28454);
#6816=VERTEX_POINT('',#28501);
#6817=VERTEX_POINT('',#28502);
#6818=VERTEX_POINT('',#28555);
#6819=VERTEX_POINT('',#28556);
#6820=VERTEX_POINT('',#28603);
#6821=VERTEX_POINT('',#28604);
#6822=VERTEX_POINT('',#28651);
#6823=VERTEX_POINT('',#28652);
#6824=VERTEX_POINT('',#28702);
#6825=VERTEX_POINT('',#28703);
#6826=VERTEX_POINT('',#28705);
#6827=VERTEX_POINT('',#28752);
#6828=VERTEX_POINT('',#28753);
#6829=VERTEX_POINT('',#28755);
#6830=VERTEX_POINT('',#28764);
#6831=VERTEX_POINT('',#28773);
#6832=VERTEX_POINT('',#28774);
#6833=VERTEX_POINT('',#28797);
#6834=VERTEX_POINT('',#28798);
#6835=VERTEX_POINT('',#28822);
#6836=VERTEX_POINT('',#28823);
#6837=VERTEX_POINT('',#28846);
#6838=VERTEX_POINT('',#28847);
#6839=VERTEX_POINT('',#28871);
#6840=VERTEX_POINT('',#28872);
#6841=VERTEX_POINT('',#28896);
#6842=VERTEX_POINT('',#28897);
#6843=VERTEX_POINT('',#28920);
#6844=VERTEX_POINT('',#28921);
#6845=VERTEX_POINT('',#28945);
#6846=VERTEX_POINT('',#28946);
#6847=VERTEX_POINT('',#28970);
#6848=VERTEX_POINT('',#28971);
#6849=VERTEX_POINT('',#28994);
#6850=VERTEX_POINT('',#28995);
#6851=VERTEX_POINT('',#29019);
#6852=VERTEX_POINT('',#29020);
#6853=VERTEX_POINT('',#29044);
#6854=VERTEX_POINT('',#29045);
#6855=VERTEX_POINT('',#29068);
#6856=VERTEX_POINT('',#29069);
#6857=VERTEX_POINT('',#29093);
#6858=VERTEX_POINT('',#29094);
#6859=VERTEX_POINT('',#29118);
#6860=VERTEX_POINT('',#29119);
#6861=VERTEX_POINT('',#29142);
#6862=VERTEX_POINT('',#29143);
#6863=VERTEX_POINT('',#29167);
#6864=VERTEX_POINT('',#29168);
#6865=VERTEX_POINT('',#29191);
#6866=VERTEX_POINT('',#29192);
#6867=VERTEX_POINT('',#29216);
#6868=VERTEX_POINT('',#29217);
#6869=VERTEX_POINT('',#29240);
#6870=VERTEX_POINT('',#29241);
#6871=VERTEX_POINT('',#29265);
#6872=VERTEX_POINT('',#29266);
#6873=VERTEX_POINT('',#29290);
#6874=VERTEX_POINT('',#29291);
#6875=VERTEX_POINT('',#29314);
#6876=VERTEX_POINT('',#29315);
#6877=VERTEX_POINT('',#29317);
#6878=VERTEX_POINT('',#29319);
#6879=VERTEX_POINT('',#29323);
#6880=VERTEX_POINT('',#29325);
#6881=VERTEX_POINT('',#29329);
#6882=VERTEX_POINT('',#29331);
#6883=VERTEX_POINT('',#29339);
#6884=VERTEX_POINT('',#29341);
#6885=VERTEX_POINT('',#29953);
#6886=VERTEX_POINT('',#30013);
#6887=VERTEX_POINT('',#30079);
#6888=VERTEX_POINT('',#30082);
#6889=VERTEX_POINT('',#30812);
#6890=VERTEX_POINT('',#30813);
#6891=VERTEX_POINT('',#30817);
#6892=VERTEX_POINT('',#30819);
#6893=VERTEX_POINT('',#30825);
#6894=VERTEX_POINT('',#30829);
#6895=VERTEX_POINT('',#30835);
#6896=VERTEX_POINT('',#30836);
#6897=VERTEX_POINT('',#30840);
#6898=VERTEX_POINT('',#30842);
#6899=VERTEX_POINT('',#30848);
#6900=VERTEX_POINT('',#30852);
#6901=VERTEX_POINT('',#30858);
#6902=VERTEX_POINT('',#30859);
#6903=VERTEX_POINT('',#30863);
#6904=VERTEX_POINT('',#30865);
#6905=VERTEX_POINT('',#30871);
#6906=VERTEX_POINT('',#30875);
#6907=VERTEX_POINT('',#30881);
#6908=VERTEX_POINT('',#30882);
#6909=VERTEX_POINT('',#30886);
#6910=VERTEX_POINT('',#30888);
#6911=VERTEX_POINT('',#30894);
#6912=VERTEX_POINT('',#30898);
#6913=VERTEX_POINT('',#30904);
#6914=VERTEX_POINT('',#30905);
#6915=VERTEX_POINT('',#30909);
#6916=VERTEX_POINT('',#30911);
#6917=VERTEX_POINT('',#30917);
#6918=VERTEX_POINT('',#30921);
#6919=VERTEX_POINT('',#30927);
#6920=VERTEX_POINT('',#30928);
#6921=VERTEX_POINT('',#30932);
#6922=VERTEX_POINT('',#30934);
#6923=VERTEX_POINT('',#30940);
#6924=VERTEX_POINT('',#30944);
#6925=VERTEX_POINT('',#30950);
#6926=VERTEX_POINT('',#30951);
#6927=VERTEX_POINT('',#30955);
#6928=VERTEX_POINT('',#30957);
#6929=VERTEX_POINT('',#30963);
#6930=VERTEX_POINT('',#30967);
#6931=VERTEX_POINT('',#30973);
#6932=VERTEX_POINT('',#30974);
#6933=VERTEX_POINT('',#30978);
#6934=VERTEX_POINT('',#30980);
#6935=VERTEX_POINT('',#30986);
#6936=VERTEX_POINT('',#30990);
#6937=VERTEX_POINT('',#30996);
#6938=VERTEX_POINT('',#30997);
#6939=VERTEX_POINT('',#31001);
#6940=VERTEX_POINT('',#31003);
#6941=VERTEX_POINT('',#31009);
#6942=VERTEX_POINT('',#31013);
#6943=VERTEX_POINT('',#31019);
#6944=VERTEX_POINT('',#31020);
#6945=VERTEX_POINT('',#31024);
#6946=VERTEX_POINT('',#31026);
#6947=VERTEX_POINT('',#31032);
#6948=VERTEX_POINT('',#31036);
#6949=VERTEX_POINT('',#31042);
#6950=VERTEX_POINT('',#31043);
#6951=VERTEX_POINT('',#31047);
#6952=VERTEX_POINT('',#31049);
#6953=VERTEX_POINT('',#31055);
#6954=VERTEX_POINT('',#31059);
#6955=VERTEX_POINT('',#31065);
#6956=VERTEX_POINT('',#31066);
#6957=VERTEX_POINT('',#31070);
#6958=VERTEX_POINT('',#31072);
#6959=VERTEX_POINT('',#31078);
#6960=VERTEX_POINT('',#31082);
#6961=VERTEX_POINT('',#31088);
#6962=VERTEX_POINT('',#31089);
#6963=VERTEX_POINT('',#31093);
#6964=VERTEX_POINT('',#31095);
#6965=VERTEX_POINT('',#31101);
#6966=VERTEX_POINT('',#31105);
#6967=VERTEX_POINT('',#31111);
#6968=VERTEX_POINT('',#31112);
#6969=VERTEX_POINT('',#31116);
#6970=VERTEX_POINT('',#31118);
#6971=VERTEX_POINT('',#31124);
#6972=VERTEX_POINT('',#31128);
#6973=VERTEX_POINT('',#31134);
#6974=VERTEX_POINT('',#31135);
#6975=VERTEX_POINT('',#31139);
#6976=VERTEX_POINT('',#31141);
#6977=VERTEX_POINT('',#31147);
#6978=VERTEX_POINT('',#31151);
#6979=VERTEX_POINT('',#31157);
#6980=VERTEX_POINT('',#31158);
#6981=VERTEX_POINT('',#31162);
#6982=VERTEX_POINT('',#31164);
#6983=VERTEX_POINT('',#31170);
#6984=VERTEX_POINT('',#31174);
#6985=VERTEX_POINT('',#31180);
#6986=VERTEX_POINT('',#31181);
#6987=VERTEX_POINT('',#31185);
#6988=VERTEX_POINT('',#31187);
#6989=VERTEX_POINT('',#31193);
#6990=VERTEX_POINT('',#31197);
#6991=VERTEX_POINT('',#31203);
#6992=VERTEX_POINT('',#31204);
#6993=VERTEX_POINT('',#31208);
#6994=VERTEX_POINT('',#31210);
#6995=VERTEX_POINT('',#31216);
#6996=VERTEX_POINT('',#31220);
#6997=VERTEX_POINT('',#31226);
#6998=VERTEX_POINT('',#31227);
#6999=VERTEX_POINT('',#31231);
#7000=VERTEX_POINT('',#31233);
#7001=VERTEX_POINT('',#31239);
#7002=VERTEX_POINT('',#31243);
#7003=VERTEX_POINT('',#31249);
#7004=VERTEX_POINT('',#31250);
#7005=VERTEX_POINT('',#31254);
#7006=VERTEX_POINT('',#31256);
#7007=VERTEX_POINT('',#31262);
#7008=VERTEX_POINT('',#31266);
#7009=VERTEX_POINT('',#31272);
#7010=VERTEX_POINT('',#31273);
#7011=VERTEX_POINT('',#31277);
#7012=VERTEX_POINT('',#31279);
#7013=VERTEX_POINT('',#31285);
#7014=VERTEX_POINT('',#31289);
#7015=VERTEX_POINT('',#31295);
#7016=VERTEX_POINT('',#31296);
#7017=VERTEX_POINT('',#31300);
#7018=VERTEX_POINT('',#31302);
#7019=VERTEX_POINT('',#31308);
#7020=VERTEX_POINT('',#31312);
#7021=VERTEX_POINT('',#31318);
#7022=VERTEX_POINT('',#31319);
#7023=VERTEX_POINT('',#31323);
#7024=VERTEX_POINT('',#31325);
#7025=VERTEX_POINT('',#31331);
#7026=VERTEX_POINT('',#31335);
#7027=VERTEX_POINT('',#31341);
#7028=VERTEX_POINT('',#31342);
#7029=VERTEX_POINT('',#31346);
#7030=VERTEX_POINT('',#31348);
#7031=VERTEX_POINT('',#31354);
#7032=VERTEX_POINT('',#31358);
#7033=VERTEX_POINT('',#31364);
#7034=VERTEX_POINT('',#31365);
#7035=VERTEX_POINT('',#31369);
#7036=VERTEX_POINT('',#31371);
#7037=VERTEX_POINT('',#31377);
#7038=VERTEX_POINT('',#31381);
#7039=VERTEX_POINT('',#31387);
#7040=VERTEX_POINT('',#31388);
#7041=VERTEX_POINT('',#31392);
#7042=VERTEX_POINT('',#31394);
#7043=VERTEX_POINT('',#31400);
#7044=VERTEX_POINT('',#31404);
#7045=VERTEX_POINT('',#31410);
#7046=VERTEX_POINT('',#31411);
#7047=VERTEX_POINT('',#31415);
#7048=VERTEX_POINT('',#31417);
#7049=VERTEX_POINT('',#31423);
#7050=VERTEX_POINT('',#31427);
#7051=VERTEX_POINT('',#31433);
#7052=VERTEX_POINT('',#31434);
#7053=VERTEX_POINT('',#31438);
#7054=VERTEX_POINT('',#31440);
#7055=VERTEX_POINT('',#31446);
#7056=VERTEX_POINT('',#31450);
#7057=VERTEX_POINT('',#31456);
#7058=VERTEX_POINT('',#31457);
#7059=VERTEX_POINT('',#31461);
#7060=VERTEX_POINT('',#31463);
#7061=VERTEX_POINT('',#31469);
#7062=VERTEX_POINT('',#31473);
#7063=VERTEX_POINT('',#31479);
#7064=VERTEX_POINT('',#31480);
#7065=VERTEX_POINT('',#31484);
#7066=VERTEX_POINT('',#31486);
#7067=VERTEX_POINT('',#31492);
#7068=VERTEX_POINT('',#31496);
#7069=VERTEX_POINT('',#31592);
#7070=VERTEX_POINT('',#31596);
#7071=VERTEX_POINT('',#31604);
#7072=VERTEX_POINT('',#31610);
#7073=VERTEX_POINT('',#31611);
#7074=VERTEX_POINT('',#32208);
#7075=VERTEX_POINT('',#32210);
#7076=VERTEX_POINT('',#32270);
#7077=VERTEX_POINT('',#32271);
#7078=VERTEX_POINT('',#32273);
#7079=VERTEX_POINT('',#32284);
#7080=VERTEX_POINT('',#32294);
#7081=VERTEX_POINT('',#32295);
#7082=VERTEX_POINT('',#32342);
#7083=VERTEX_POINT('',#32343);
#7084=VERTEX_POINT('',#32390);
#7085=VERTEX_POINT('',#32391);
#7086=VERTEX_POINT('',#32441);
#7087=VERTEX_POINT('',#32442);
#7088=VERTEX_POINT('',#32492);
#7089=VERTEX_POINT('',#32493);
#7090=VERTEX_POINT('',#32540);
#7091=VERTEX_POINT('',#32541);
#7092=VERTEX_POINT('',#32588);
#7093=VERTEX_POINT('',#32589);
#7094=VERTEX_POINT('',#32642);
#7095=VERTEX_POINT('',#32643);
#7096=VERTEX_POINT('',#32690);
#7097=VERTEX_POINT('',#32691);
#7098=VERTEX_POINT('',#32738);
#7099=VERTEX_POINT('',#32739);
#7100=VERTEX_POINT('',#32792);
#7101=VERTEX_POINT('',#32793);
#7102=VERTEX_POINT('',#32840);
#7103=VERTEX_POINT('',#32841);
#7104=VERTEX_POINT('',#32888);
#7105=VERTEX_POINT('',#32889);
#7106=VERTEX_POINT('',#32936);
#7107=VERTEX_POINT('',#32937);
#7108=VERTEX_POINT('',#32990);
#7109=VERTEX_POINT('',#32991);
#7110=VERTEX_POINT('',#33038);
#7111=VERTEX_POINT('',#33039);
#7112=VERTEX_POINT('',#33086);
#7113=VERTEX_POINT('',#33087);
#7114=VERTEX_POINT('',#33140);
#7115=VERTEX_POINT('',#33141);
#7116=VERTEX_POINT('',#33188);
#7117=VERTEX_POINT('',#33189);
#7118=VERTEX_POINT('',#33236);
#7119=VERTEX_POINT('',#33237);
#7120=VERTEX_POINT('',#33290);
#7121=VERTEX_POINT('',#33291);
#7122=VERTEX_POINT('',#33338);
#7123=VERTEX_POINT('',#33339);
#7124=VERTEX_POINT('',#33341);
#7125=VERTEX_POINT('',#33348);
#7126=VERTEX_POINT('',#33356);
#7127=VERTEX_POINT('',#33357);
#7128=VERTEX_POINT('',#33380);
#7129=VERTEX_POINT('',#33381);
#7130=VERTEX_POINT('',#33405);
#7131=VERTEX_POINT('',#33406);
#7132=VERTEX_POINT('',#33430);
#7133=VERTEX_POINT('',#33431);
#7134=VERTEX_POINT('',#33454);
#7135=VERTEX_POINT('',#33455);
#7136=VERTEX_POINT('',#33479);
#7137=VERTEX_POINT('',#33480);
#7138=VERTEX_POINT('',#33504);
#7139=VERTEX_POINT('',#33505);
#7140=VERTEX_POINT('',#33528);
#7141=VERTEX_POINT('',#33529);
#7142=VERTEX_POINT('',#33553);
#7143=VERTEX_POINT('',#33554);
#7144=VERTEX_POINT('',#33578);
#7145=VERTEX_POINT('',#33579);
#7146=VERTEX_POINT('',#33602);
#7147=VERTEX_POINT('',#33603);
#7148=VERTEX_POINT('',#33626);
#7149=VERTEX_POINT('',#33627);
#7150=VERTEX_POINT('',#33651);
#7151=VERTEX_POINT('',#33652);
#7152=VERTEX_POINT('',#33676);
#7153=VERTEX_POINT('',#33677);
#7154=VERTEX_POINT('',#33700);
#7155=VERTEX_POINT('',#33701);
#7156=VERTEX_POINT('',#33725);
#7157=VERTEX_POINT('',#33726);
#7158=VERTEX_POINT('',#33750);
#7159=VERTEX_POINT('',#33751);
#7160=VERTEX_POINT('',#33774);
#7161=VERTEX_POINT('',#33775);
#7162=VERTEX_POINT('',#33799);
#7163=VERTEX_POINT('',#33800);
#7164=VERTEX_POINT('',#33823);
#7165=VERTEX_POINT('',#33824);
#7166=VERTEX_POINT('',#33848);
#7167=VERTEX_POINT('',#33849);
#7168=VERTEX_POINT('',#33872);
#7169=VERTEX_POINT('',#33925);
#7170=VERTEX_POINT('',#33927);
#7171=VERTEX_POINT('',#34576);
#7172=VERTEX_POINT('',#34639);
#7173=VERTEX_POINT('',#34642);
#7174=VERTEX_POINT('',#35298);
#7175=VERTEX_POINT('',#35304);
#7176=VERTEX_POINT('',#35305);
#7177=VERTEX_POINT('',#35307);
#7178=VERTEX_POINT('',#35309);
#7179=VERTEX_POINT('',#35311);
#7180=VERTEX_POINT('',#35313);
#7181=VERTEX_POINT('',#35315);
#7182=VERTEX_POINT('',#35317);
#7183=VERTEX_POINT('',#35319);
#7184=VERTEX_POINT('',#35321);
#7185=VERTEX_POINT('',#35323);
#7186=VERTEX_POINT('',#35325);
#7187=VERTEX_POINT('',#35327);
#7188=VERTEX_POINT('',#35329);
#7189=VERTEX_POINT('',#35331);
#7190=VERTEX_POINT('',#35333);
#7191=VERTEX_POINT('',#35335);
#7192=VERTEX_POINT('',#35337);
#7193=VERTEX_POINT('',#35339);
#7194=VERTEX_POINT('',#35341);
#7195=VERTEX_POINT('',#35343);
#7196=VERTEX_POINT('',#35345);
#7197=VERTEX_POINT('',#35347);
#7198=VERTEX_POINT('',#35349);
#7199=VERTEX_POINT('',#35351);
#7200=VERTEX_POINT('',#35353);
#7201=VERTEX_POINT('',#35355);
#7202=VERTEX_POINT('',#35357);
#7203=VERTEX_POINT('',#35359);
#7204=VERTEX_POINT('',#35361);
#7205=VERTEX_POINT('',#35363);
#7206=VERTEX_POINT('',#35365);
#7207=VERTEX_POINT('',#35367);
#7208=VERTEX_POINT('',#35369);
#7209=VERTEX_POINT('',#35371);
#7210=VERTEX_POINT('',#35373);
#7211=VERTEX_POINT('',#35375);
#7212=VERTEX_POINT('',#35377);
#7213=VERTEX_POINT('',#35379);
#7214=VERTEX_POINT('',#35381);
#7215=VERTEX_POINT('',#35383);
#7216=VERTEX_POINT('',#35385);
#7217=VERTEX_POINT('',#35387);
#7218=VERTEX_POINT('',#35389);
#7219=VERTEX_POINT('',#35391);
#7220=VERTEX_POINT('',#35393);
#7221=VERTEX_POINT('',#35395);
#7222=VERTEX_POINT('',#35397);
#7223=VERTEX_POINT('',#35399);
#7224=VERTEX_POINT('',#35401);
#7225=VERTEX_POINT('',#35403);
#7226=VERTEX_POINT('',#35405);
#7227=VERTEX_POINT('',#35407);
#7228=VERTEX_POINT('',#35409);
#7229=VERTEX_POINT('',#35411);
#7230=VERTEX_POINT('',#35413);
#7231=VERTEX_POINT('',#35415);
#7232=VERTEX_POINT('',#35417);
#7233=VERTEX_POINT('',#35419);
#7234=VERTEX_POINT('',#35421);
#7235=VERTEX_POINT('',#35423);
#7236=VERTEX_POINT('',#35425);
#7237=VERTEX_POINT('',#35427);
#7238=VERTEX_POINT('',#35429);
#7239=VERTEX_POINT('',#35431);
#7240=VERTEX_POINT('',#35433);
#7241=VERTEX_POINT('',#35435);
#7242=VERTEX_POINT('',#35437);
#7243=VERTEX_POINT('',#35439);
#7244=VERTEX_POINT('',#35441);
#7245=VERTEX_POINT('',#35443);
#7246=VERTEX_POINT('',#35445);
#7247=VERTEX_POINT('',#35447);
#7248=VERTEX_POINT('',#35449);
#7249=VERTEX_POINT('',#35451);
#7250=VERTEX_POINT('',#35453);
#7251=VERTEX_POINT('',#35455);
#7252=VERTEX_POINT('',#35457);
#7253=VERTEX_POINT('',#35459);
#7254=VERTEX_POINT('',#35461);
#7255=VERTEX_POINT('',#35463);
#7256=VERTEX_POINT('',#35465);
#7257=VERTEX_POINT('',#35467);
#7258=VERTEX_POINT('',#35469);
#7259=VERTEX_POINT('',#35471);
#7260=VERTEX_POINT('',#35473);
#7261=VERTEX_POINT('',#35475);
#7262=VERTEX_POINT('',#35477);
#7263=VERTEX_POINT('',#35479);
#7264=VERTEX_POINT('',#35481);
#7265=VERTEX_POINT('',#35483);
#7266=VERTEX_POINT('',#35485);
#7267=VERTEX_POINT('',#35487);
#7268=VERTEX_POINT('',#35489);
#7269=VERTEX_POINT('',#35491);
#7270=VERTEX_POINT('',#35493);
#7271=VERTEX_POINT('',#35495);
#7272=VERTEX_POINT('',#35497);
#7273=VERTEX_POINT('',#35499);
#7274=VERTEX_POINT('',#35501);
#7275=VERTEX_POINT('',#35503);
#7276=VERTEX_POINT('',#35505);
#7277=VERTEX_POINT('',#35507);
#7278=VERTEX_POINT('',#35509);
#7279=VERTEX_POINT('',#35511);
#7280=VERTEX_POINT('',#35513);
#7281=VERTEX_POINT('',#35515);
#7282=VERTEX_POINT('',#35517);
#7283=VERTEX_POINT('',#35521);
#7284=VERTEX_POINT('',#35522);
#7285=VERTEX_POINT('',#35526);
#7286=VERTEX_POINT('',#35530);
#7287=VERTEX_POINT('',#35534);
#7288=VERTEX_POINT('',#35538);
#7289=VERTEX_POINT('',#35545);
#7290=VERTEX_POINT('',#35546);
#7291=VERTEX_POINT('',#35548);
#7292=VERTEX_POINT('',#35553);
#7293=VERTEX_POINT('',#35557);
#7294=VERTEX_POINT('',#35562);
#7295=VERTEX_POINT('',#35566);
#7296=VERTEX_POINT('',#35571);
#7297=VERTEX_POINT('',#35575);
#7298=VERTEX_POINT('',#35580);
#7299=VERTEX_POINT('',#35584);
#7300=VERTEX_POINT('',#35589);
#7301=VERTEX_POINT('',#35593);
#7302=VERTEX_POINT('',#35598);
#7303=VERTEX_POINT('',#35604);
#7304=VERTEX_POINT('',#35606);
#7305=VERTEX_POINT('',#35610);
#7306=VERTEX_POINT('',#35614);
#7307=VERTEX_POINT('',#35618);
#7308=VERTEX_POINT('',#35622);
#7309=VERTEX_POINT('',#35626);
#7310=VERTEX_POINT('',#35630);
#7311=VERTEX_POINT('',#35634);
#7312=VERTEX_POINT('',#35638);
#7313=VERTEX_POINT('',#35649);
#7314=VERTEX_POINT('',#35657);
#7315=VERTEX_POINT('',#35670);
#7316=VERTEX_POINT('',#35671);
#7317=VERTEX_POINT('',#35678);
#7318=VERTEX_POINT('',#35684);
#7319=VERTEX_POINT('',#35685);
#7320=VERTEX_POINT('',#35692);
#7321=VERTEX_POINT('',#35698);
#7322=VERTEX_POINT('',#35699);
#7323=VERTEX_POINT('',#35706);
#7324=VERTEX_POINT('',#35712);
#7325=VERTEX_POINT('',#35713);
#7326=VERTEX_POINT('',#35720);
#7327=VERTEX_POINT('',#35726);
#7328=VERTEX_POINT('',#35727);
#7329=VERTEX_POINT('',#35734);
#7330=VERTEX_POINT('',#35740);
#7331=VERTEX_POINT('',#35741);
#7332=VERTEX_POINT('',#35748);
#7333=VERTEX_POINT('',#35754);
#7334=VERTEX_POINT('',#35755);
#7335=VERTEX_POINT('',#35762);
#7336=VERTEX_POINT('',#35768);
#7337=VERTEX_POINT('',#35769);
#7338=VERTEX_POINT('',#35776);
#7339=VERTEX_POINT('',#35782);
#7340=VERTEX_POINT('',#35783);
#7341=VERTEX_POINT('',#35790);
#7342=VERTEX_POINT('',#35796);
#7343=VERTEX_POINT('',#35797);
#7344=VERTEX_POINT('',#35804);
#7345=VERTEX_POINT('',#35810);
#7346=VERTEX_POINT('',#35811);
#7347=VERTEX_POINT('',#35818);
#7348=VERTEX_POINT('',#35824);
#7349=VERTEX_POINT('',#35825);
#7350=VERTEX_POINT('',#35832);
#7351=VERTEX_POINT('',#35838);
#7352=VERTEX_POINT('',#35839);
#7353=VERTEX_POINT('',#35846);
#7354=VERTEX_POINT('',#35852);
#7355=VERTEX_POINT('',#35853);
#7356=VERTEX_POINT('',#35860);
#7357=VERTEX_POINT('',#35866);
#7358=VERTEX_POINT('',#35867);
#7359=VERTEX_POINT('',#35874);
#7360=VERTEX_POINT('',#35880);
#7361=VERTEX_POINT('',#35881);
#7362=VERTEX_POINT('',#35888);
#7363=VERTEX_POINT('',#35894);
#7364=VERTEX_POINT('',#35895);
#7365=VERTEX_POINT('',#35902);
#7366=VERTEX_POINT('',#35908);
#7367=VERTEX_POINT('',#35909);
#7368=VERTEX_POINT('',#35916);
#7369=VERTEX_POINT('',#35922);
#7370=VERTEX_POINT('',#35923);
#7371=VERTEX_POINT('',#35930);
#7372=VERTEX_POINT('',#35936);
#7373=VERTEX_POINT('',#35937);
#7374=VERTEX_POINT('',#35944);
#7375=VERTEX_POINT('',#35950);
#7376=VERTEX_POINT('',#35951);
#7377=VERTEX_POINT('',#35958);
#7378=VERTEX_POINT('',#35964);
#7379=VERTEX_POINT('',#35965);
#7380=VERTEX_POINT('',#35972);
#7381=VERTEX_POINT('',#35978);
#7382=VERTEX_POINT('',#35979);
#7383=VERTEX_POINT('',#35986);
#7384=VERTEX_POINT('',#35992);
#7385=VERTEX_POINT('',#35993);
#7386=VERTEX_POINT('',#36000);
#7387=VERTEX_POINT('',#36006);
#7388=VERTEX_POINT('',#36007);
#7389=VERTEX_POINT('',#36014);
#7390=VERTEX_POINT('',#36020);
#7391=VERTEX_POINT('',#36021);
#7392=VERTEX_POINT('',#36028);
#7393=VERTEX_POINT('',#36034);
#7394=VERTEX_POINT('',#36035);
#7395=VERTEX_POINT('',#36042);
#7396=VERTEX_POINT('',#36048);
#7397=VERTEX_POINT('',#36049);
#7398=VERTEX_POINT('',#36056);
#7399=VERTEX_POINT('',#36062);
#7400=VERTEX_POINT('',#36063);
#7401=VERTEX_POINT('',#36070);
#7402=VERTEX_POINT('',#36076);
#7403=VERTEX_POINT('',#36077);
#7404=VERTEX_POINT('',#36084);
#7405=VERTEX_POINT('',#36090);
#7406=VERTEX_POINT('',#36091);
#7407=VERTEX_POINT('',#36098);
#7408=VERTEX_POINT('',#36104);
#7409=VERTEX_POINT('',#36105);
#7410=VERTEX_POINT('',#36112);
#7411=VERTEX_POINT('',#36118);
#7412=VERTEX_POINT('',#36119);
#7413=VERTEX_POINT('',#36126);
#7414=VERTEX_POINT('',#36132);
#7415=VERTEX_POINT('',#36133);
#7416=VERTEX_POINT('',#36140);
#7417=VERTEX_POINT('',#36146);
#7418=VERTEX_POINT('',#36147);
#7419=VERTEX_POINT('',#36154);
#7420=VERTEX_POINT('',#36160);
#7421=VERTEX_POINT('',#36161);
#7422=VERTEX_POINT('',#36168);
#7423=VERTEX_POINT('',#36246);
#7424=VERTEX_POINT('',#36251);
#7425=VERTEX_POINT('',#36257);
#7426=VERTEX_POINT('',#36258);
#7427=VERTEX_POINT('',#36260);
#7428=VERTEX_POINT('',#36271);
#7429=VERTEX_POINT('',#36281);
#7430=VERTEX_POINT('',#36282);
#7431=VERTEX_POINT('',#36329);
#7432=VERTEX_POINT('',#36330);
#7433=VERTEX_POINT('',#36377);
#7434=VERTEX_POINT('',#36378);
#7435=VERTEX_POINT('',#36431);
#7436=VERTEX_POINT('',#36432);
#7437=VERTEX_POINT('',#36479);
#7438=VERTEX_POINT('',#36480);
#7439=VERTEX_POINT('',#36527);
#7440=VERTEX_POINT('',#36528);
#7441=VERTEX_POINT('',#36581);
#7442=VERTEX_POINT('',#36582);
#7443=VERTEX_POINT('',#36629);
#7444=VERTEX_POINT('',#36630);
#7445=VERTEX_POINT('',#36677);
#7446=VERTEX_POINT('',#36678);
#7447=VERTEX_POINT('',#36725);
#7448=VERTEX_POINT('',#36726);
#7449=VERTEX_POINT('',#36779);
#7450=VERTEX_POINT('',#36780);
#7451=VERTEX_POINT('',#36782);
#7452=VERTEX_POINT('',#36789);
#7453=VERTEX_POINT('',#36797);
#7454=VERTEX_POINT('',#36798);
#7455=VERTEX_POINT('',#36822);
#7456=VERTEX_POINT('',#36823);
#7457=VERTEX_POINT('',#36847);
#7458=VERTEX_POINT('',#36848);
#7459=VERTEX_POINT('',#36871);
#7460=VERTEX_POINT('',#36872);
#7461=VERTEX_POINT('',#36895);
#7462=VERTEX_POINT('',#36896);
#7463=VERTEX_POINT('',#36920);
#7464=VERTEX_POINT('',#36921);
#7465=VERTEX_POINT('',#36945);
#7466=VERTEX_POINT('',#36946);
#7467=VERTEX_POINT('',#36969);
#7468=VERTEX_POINT('',#36970);
#7469=VERTEX_POINT('',#36994);
#7470=VERTEX_POINT('',#36995);
#7471=VERTEX_POINT('',#37019);
#7472=VERTEX_POINT('',#37020);
#7473=VERTEX_POINT('',#37342);
#7474=VERTEX_POINT('',#37417);
#7475=VERTEX_POINT('',#37480);
#7476=VERTEX_POINT('',#37483);
#7477=VERTEX_POINT('',#37849);
#7478=VERTEX_POINT('',#37919);
#7479=VERTEX_POINT('',#37920);
#7480=VERTEX_POINT('',#37924);
#7481=VERTEX_POINT('',#37926);
#7482=VERTEX_POINT('',#37932);
#7483=VERTEX_POINT('',#37936);
#7484=VERTEX_POINT('',#37942);
#7485=VERTEX_POINT('',#37943);
#7486=VERTEX_POINT('',#37947);
#7487=VERTEX_POINT('',#37949);
#7488=VERTEX_POINT('',#37955);
#7489=VERTEX_POINT('',#37959);
#7490=VERTEX_POINT('',#37965);
#7491=VERTEX_POINT('',#37966);
#7492=VERTEX_POINT('',#37970);
#7493=VERTEX_POINT('',#37972);
#7494=VERTEX_POINT('',#37978);
#7495=VERTEX_POINT('',#37982);
#7496=VERTEX_POINT('',#37988);
#7497=VERTEX_POINT('',#37989);
#7498=VERTEX_POINT('',#37993);
#7499=VERTEX_POINT('',#37995);
#7500=VERTEX_POINT('',#38001);
#7501=VERTEX_POINT('',#38005);
#7502=VERTEX_POINT('',#38011);
#7503=VERTEX_POINT('',#38012);
#7504=VERTEX_POINT('',#38016);
#7505=VERTEX_POINT('',#38018);
#7506=VERTEX_POINT('',#38024);
#7507=VERTEX_POINT('',#38028);
#7508=VERTEX_POINT('',#38034);
#7509=VERTEX_POINT('',#38035);
#7510=VERTEX_POINT('',#38039);
#7511=VERTEX_POINT('',#38041);
#7512=VERTEX_POINT('',#38047);
#7513=VERTEX_POINT('',#38051);
#7514=VERTEX_POINT('',#38057);
#7515=VERTEX_POINT('',#38058);
#7516=VERTEX_POINT('',#38062);
#7517=VERTEX_POINT('',#38064);
#7518=VERTEX_POINT('',#38070);
#7519=VERTEX_POINT('',#38074);
#7520=VERTEX_POINT('',#38080);
#7521=VERTEX_POINT('',#38081);
#7522=VERTEX_POINT('',#38085);
#7523=VERTEX_POINT('',#38087);
#7524=VERTEX_POINT('',#38093);
#7525=VERTEX_POINT('',#38097);
#7526=VERTEX_POINT('',#38103);
#7527=VERTEX_POINT('',#38104);
#7528=VERTEX_POINT('',#38108);
#7529=VERTEX_POINT('',#38110);
#7530=VERTEX_POINT('',#38116);
#7531=VERTEX_POINT('',#38120);
#7532=VERTEX_POINT('',#38126);
#7533=VERTEX_POINT('',#38127);
#7534=VERTEX_POINT('',#38131);
#7535=VERTEX_POINT('',#38133);
#7536=VERTEX_POINT('',#38139);
#7537=VERTEX_POINT('',#38143);
#7538=VERTEX_POINT('',#38149);
#7539=VERTEX_POINT('',#38150);
#7540=VERTEX_POINT('',#38154);
#7541=VERTEX_POINT('',#38156);
#7542=VERTEX_POINT('',#38162);
#7543=VERTEX_POINT('',#38166);
#7544=VERTEX_POINT('',#38172);
#7545=VERTEX_POINT('',#38173);
#7546=VERTEX_POINT('',#38177);
#7547=VERTEX_POINT('',#38179);
#7548=VERTEX_POINT('',#38185);
#7549=VERTEX_POINT('',#38189);
#7550=VERTEX_POINT('',#38195);
#7551=VERTEX_POINT('',#38196);
#7552=VERTEX_POINT('',#38200);
#7553=VERTEX_POINT('',#38202);
#7554=VERTEX_POINT('',#38208);
#7555=VERTEX_POINT('',#38212);
#7556=VERTEX_POINT('',#38218);
#7557=VERTEX_POINT('',#38219);
#7558=VERTEX_POINT('',#38223);
#7559=VERTEX_POINT('',#38225);
#7560=VERTEX_POINT('',#38231);
#7561=VERTEX_POINT('',#38235);
#7562=VERTEX_POINT('',#38241);
#7563=VERTEX_POINT('',#38242);
#7564=VERTEX_POINT('',#38246);
#7565=VERTEX_POINT('',#38248);
#7566=VERTEX_POINT('',#38254);
#7567=VERTEX_POINT('',#38258);
#7568=VERTEX_POINT('',#38264);
#7569=VERTEX_POINT('',#38265);
#7570=VERTEX_POINT('',#38269);
#7571=VERTEX_POINT('',#38271);
#7572=VERTEX_POINT('',#38277);
#7573=VERTEX_POINT('',#38281);
#7574=VERTEX_POINT('',#38287);
#7575=VERTEX_POINT('',#38288);
#7576=VERTEX_POINT('',#38292);
#7577=VERTEX_POINT('',#38294);
#7578=VERTEX_POINT('',#38300);
#7579=VERTEX_POINT('',#38304);
#7580=VERTEX_POINT('',#38310);
#7581=VERTEX_POINT('',#38311);
#7582=VERTEX_POINT('',#38315);
#7583=VERTEX_POINT('',#38317);
#7584=VERTEX_POINT('',#38323);
#7585=VERTEX_POINT('',#38327);
#7586=VERTEX_POINT('',#38333);
#7587=VERTEX_POINT('',#38334);
#7588=VERTEX_POINT('',#38338);
#7589=VERTEX_POINT('',#38340);
#7590=VERTEX_POINT('',#38346);
#7591=VERTEX_POINT('',#38350);
#7592=VERTEX_POINT('',#38356);
#7593=VERTEX_POINT('',#38357);
#7594=VERTEX_POINT('',#38361);
#7595=VERTEX_POINT('',#38363);
#7596=VERTEX_POINT('',#38369);
#7597=VERTEX_POINT('',#38373);
#7598=VERTEX_POINT('',#38379);
#7599=VERTEX_POINT('',#38380);
#7600=VERTEX_POINT('',#38384);
#7601=VERTEX_POINT('',#38386);
#7602=VERTEX_POINT('',#38392);
#7603=VERTEX_POINT('',#38396);
#7604=VERTEX_POINT('',#38402);
#7605=VERTEX_POINT('',#38403);
#7606=VERTEX_POINT('',#38407);
#7607=VERTEX_POINT('',#38409);
#7608=VERTEX_POINT('',#38415);
#7609=VERTEX_POINT('',#38419);
#7610=VERTEX_POINT('',#38425);
#7611=VERTEX_POINT('',#38426);
#7612=VERTEX_POINT('',#38430);
#7613=VERTEX_POINT('',#38432);
#7614=VERTEX_POINT('',#38438);
#7615=VERTEX_POINT('',#38442);
#7616=VERTEX_POINT('',#38448);
#7617=VERTEX_POINT('',#38449);
#7618=VERTEX_POINT('',#38453);
#7619=VERTEX_POINT('',#38455);
#7620=VERTEX_POINT('',#38461);
#7621=VERTEX_POINT('',#38465);
#7622=VERTEX_POINT('',#38543);
#7623=VERTEX_POINT('',#38547);
#7624=VERTEX_POINT('',#38555);
#7625=EDGE_CURVE('',#6102,#6103,#3654,.T.);
#7626=EDGE_CURVE('',#6103,#6104,#3655,.T.);
#7627=EDGE_CURVE('',#6104,#6105,#3656,.T.);
#7628=EDGE_CURVE('',#6105,#6106,#3657,.T.);
#7629=EDGE_CURVE('',#6106,#6107,#3658,.T.);
#7630=EDGE_CURVE('',#6107,#6102,#3659,.T.);
#7631=EDGE_CURVE('',#6108,#6105,#3660,.T.);
#7632=EDGE_CURVE('',#6109,#6108,#3661,.T.);
#7633=EDGE_CURVE('',#6110,#6109,#3662,.T.);
#7634=EDGE_CURVE('',#6110,#6106,#3663,.T.);
#7635=EDGE_CURVE('',#6104,#6111,#3664,.T.);
#7636=EDGE_CURVE('',#6112,#6111,#3665,.T.);
#7637=EDGE_CURVE('',#6113,#6112,#3666,.T.);
#7638=EDGE_CURVE('',#6108,#6113,#3667,.T.);
#7639=EDGE_CURVE('',#6114,#6103,#3668,.T.);
#7640=EDGE_CURVE('',#6111,#6114,#3669,.T.);
#7641=EDGE_CURVE('',#6114,#6115,#3670,.T.);
#7642=EDGE_CURVE('',#6115,#6116,#3671,.T.);
#7643=EDGE_CURVE('',#6116,#6117,#3672,.T.);
#7644=EDGE_CURVE('',#6117,#6112,#3673,.T.);
#7645=EDGE_CURVE('',#6117,#6118,#3674,.T.);
#7646=EDGE_CURVE('',#6118,#6119,#3675,.T.);
#7647=EDGE_CURVE('',#6113,#6119,#3676,.T.);
#7648=EDGE_CURVE('',#6120,#6121,#3677,.T.);
#7649=EDGE_CURVE('',#6121,#6122,#3678,.T.);
#7650=EDGE_CURVE('',#6122,#6123,#3679,.T.);
#7651=EDGE_CURVE('',#6123,#6124,#3680,.T.);
#7652=EDGE_CURVE('',#6124,#6125,#3681,.T.);
#7653=EDGE_CURVE('',#6125,#6120,#3682,.T.);
#7654=EDGE_CURVE('',#6126,#6121,#3683,.T.);
#7655=EDGE_CURVE('',#6127,#6126,#3684,.T.);
#7656=EDGE_CURVE('',#6122,#6127,#3685,.T.);
#7657=EDGE_CURVE('',#6128,#6120,#3686,.T.);
#7658=EDGE_CURVE('',#6129,#6128,#3687,.T.);
#7659=EDGE_CURVE('',#6126,#6129,#3688,.T.);
#7660=EDGE_CURVE('',#6125,#6130,#3689,.T.);
#7661=EDGE_CURVE('',#6130,#6131,#3690,.T.);
#7662=EDGE_CURVE('',#6128,#6131,#3691,.T.);
#7663=EDGE_CURVE('',#6132,#6133,#3692,.T.);
#7664=EDGE_CURVE('',#6133,#6134,#3693,.T.);
#7665=EDGE_CURVE('',#6134,#6135,#3694,.T.);
#7666=EDGE_CURVE('',#6135,#6136,#3695,.T.);
#7667=EDGE_CURVE('',#6136,#6137,#3696,.T.);
#7668=EDGE_CURVE('',#6137,#6132,#3697,.T.);
#7669=EDGE_CURVE('',#6134,#6138,#3698,.T.);
#7670=EDGE_CURVE('',#6138,#6139,#3699,.T.);
#7671=EDGE_CURVE('',#6140,#6139,#3700,.T.);
#7672=EDGE_CURVE('',#6140,#6135,#3701,.T.);
#7673=EDGE_CURVE('',#6141,#6133,#3702,.T.);
#7674=EDGE_CURVE('',#6138,#6141,#3703,.T.);
#7675=EDGE_CURVE('',#6132,#6142,#3704,.T.);
#7676=EDGE_CURVE('',#6142,#6143,#3705,.T.);
#7677=EDGE_CURVE('',#6143,#6141,#3706,.T.);
#7678=EDGE_CURVE('',#6144,#6145,#3707,.T.);
#7679=EDGE_CURVE('',#6145,#6146,#3708,.T.);
#7680=EDGE_CURVE('',#6146,#6147,#3709,.T.);
#7681=EDGE_CURVE('',#6147,#6148,#3710,.T.);
#7682=EDGE_CURVE('',#6148,#6149,#3711,.T.);
#7683=EDGE_CURVE('',#6149,#6144,#3712,.T.);
#7684=EDGE_CURVE('',#6146,#6150,#3713,.T.);
#7685=EDGE_CURVE('',#6151,#6150,#3714,.T.);
#7686=EDGE_CURVE('',#6151,#6152,#3715,.T.);
#7687=EDGE_CURVE('',#6152,#6153,#3716,.T.);
#7688=EDGE_CURVE('',#6153,#6147,#3717,.T.);
#7689=EDGE_CURVE('',#6154,#6145,#3718,.T.);
#7690=EDGE_CURVE('',#6150,#6154,#3719,.T.);
#7691=EDGE_CURVE('',#6155,#6144,#3720,.T.);
#7692=EDGE_CURVE('',#6156,#6155,#3721,.T.);
#7693=EDGE_CURVE('',#6156,#6157,#3722,.T.);
#7694=EDGE_CURVE('',#6154,#6157,#3723,.T.);
#7695=EDGE_CURVE('',#6157,#6158,#3724,.T.);
#7696=EDGE_CURVE('',#6158,#6159,#3725,.T.);
#7697=EDGE_CURVE('',#6159,#6151,#3726,.T.);
#7698=EDGE_CURVE('',#6160,#6160,#1205,.T.);
#7699=EDGE_CURVE('',#6160,#6161,#3727,.T.);
#7700=EDGE_CURVE('',#6161,#6161,#1206,.T.);
#7701=EDGE_CURVE('',#6160,#6162,#3728,.T.);
#7702=EDGE_CURVE('',#6162,#6162,#1207,.T.);
#7703=EDGE_CURVE('',#6163,#6163,#1208,.T.);
#7704=EDGE_CURVE('',#6162,#6164,#3729,.T.);
#7705=EDGE_CURVE('',#6164,#6164,#1209,.T.);
#7706=EDGE_CURVE('',#6164,#6165,#3730,.T.);
#7707=EDGE_CURVE('',#6165,#6165,#1210,.T.);
#7708=EDGE_CURVE('',#6166,#6166,#510,.T.);
#7709=EDGE_CURVE('',#6166,#6167,#3731,.T.);
#7710=EDGE_CURVE('',#6167,#6168,#511,.T.);
#7711=EDGE_CURVE('',#6168,#6167,#512,.T.);
#7712=EDGE_CURVE('',#6168,#6169,#3732,.T.);
#7713=EDGE_CURVE('',#6170,#6169,#513,.T.);
#7714=EDGE_CURVE('',#6169,#6170,#514,.T.);
#7715=EDGE_CURVE('',#6171,#6172,#3733,.T.);
#7716=EDGE_CURVE('',#6172,#6173,#3734,.T.);
#7717=EDGE_CURVE('',#6173,#6174,#3735,.T.);
#7718=EDGE_CURVE('',#6174,#6175,#3736,.T.);
#7719=EDGE_CURVE('',#6175,#6176,#3737,.T.);
#7720=EDGE_CURVE('',#6176,#6171,#3738,.T.);
#7721=EDGE_CURVE('',#6177,#6175,#3739,.T.);
#7722=EDGE_CURVE('',#6177,#6178,#3740,.T.);
#7723=EDGE_CURVE('',#6176,#6178,#3741,.T.);
#7724=EDGE_CURVE('',#6179,#6174,#3742,.T.);
#7725=EDGE_CURVE('',#6180,#6179,#3743,.T.);
#7726=EDGE_CURVE('',#6181,#6180,#3744,.T.);
#7727=EDGE_CURVE('',#6177,#6181,#3745,.T.);
#7728=EDGE_CURVE('',#6173,#6182,#3746,.T.);
#7729=EDGE_CURVE('',#6182,#6183,#3747,.T.);
#7730=EDGE_CURVE('',#6183,#6179,#3748,.T.);
#7731=EDGE_CURVE('',#6184,#6185,#3749,.T.);
#7732=EDGE_CURVE('',#6185,#6186,#3750,.T.);
#7733=EDGE_CURVE('',#6186,#6187,#3751,.T.);
#7734=EDGE_CURVE('',#6187,#6188,#3752,.T.);
#7735=EDGE_CURVE('',#6188,#6189,#3753,.T.);
#7736=EDGE_CURVE('',#6189,#6184,#3754,.T.);
#7737=EDGE_CURVE('',#6186,#6190,#3755,.T.);
#7738=EDGE_CURVE('',#6191,#6190,#3756,.T.);
#7739=EDGE_CURVE('',#6191,#6192,#3757,.T.);
#7740=EDGE_CURVE('',#6192,#6187,#3758,.T.);
#7741=EDGE_CURVE('',#6193,#6185,#3759,.T.);
#7742=EDGE_CURVE('',#6190,#6193,#3760,.T.);
#7743=EDGE_CURVE('',#6184,#6194,#3761,.T.);
#7744=EDGE_CURVE('',#6194,#6195,#3762,.T.);
#7745=EDGE_CURVE('',#6193,#6195,#3763,.T.);
#7746=EDGE_CURVE('',#6196,#6197,#3764,.T.);
#7747=EDGE_CURVE('',#6197,#6183,#1211,.T.);
#7748=EDGE_CURVE('',#6182,#6196,#1212,.T.);
#7749=EDGE_CURVE('',#6198,#6199,#3765,.T.);
#7750=EDGE_CURVE('',#6199,#6197,#3766,.T.);
#7751=EDGE_CURVE('',#6196,#6198,#3767,.T.);
#7752=EDGE_CURVE('',#6195,#6199,#1213,.T.);
#7753=EDGE_CURVE('',#6198,#6193,#1214,.T.);
#7754=EDGE_CURVE('',#6189,#6200,#3768,.T.);
#7755=EDGE_CURVE('',#6200,#6201,#3769,.T.);
#7756=EDGE_CURVE('',#6202,#6201,#3770,.T.);
#7757=EDGE_CURVE('',#6202,#6194,#3771,.T.);
#7758=EDGE_CURVE('',#6203,#6188,#3772,.T.);
#7759=EDGE_CURVE('',#6200,#6203,#3773,.T.);
#7760=EDGE_CURVE('',#6198,#6204,#3774,.T.);
#7761=EDGE_CURVE('',#6190,#6204,#1215,.T.);
#7762=EDGE_CURVE('',#6205,#6196,#3775,.T.);
#7763=EDGE_CURVE('',#6204,#6205,#3776,.T.);
#7764=EDGE_CURVE('',#6182,#6206,#3777,.T.);
#7765=EDGE_CURVE('',#6205,#6206,#1216,.T.);
#7766=EDGE_CURVE('',#6206,#6172,#3778,.T.);
#7767=EDGE_CURVE('',#6202,#6207,#3779,.T.);
#7768=EDGE_CURVE('',#6207,#6208,#3780,.T.);
#7769=EDGE_CURVE('',#6208,#6209,#3781,.T.);
#7770=EDGE_CURVE('',#6209,#6202,#3782,.T.);
#7771=EDGE_CURVE('',#6210,#6211,#3783,.T.);
#7772=EDGE_CURVE('',#6211,#6209,#1217,.T.);
#7773=EDGE_CURVE('',#6208,#6210,#1218,.T.);
#7774=EDGE_CURVE('',#6212,#6213,#3784,.T.);
#7775=EDGE_CURVE('',#6213,#6211,#3785,.T.);
#7776=EDGE_CURVE('',#6210,#6212,#3786,.T.);
#7777=EDGE_CURVE('',#6214,#6215,#3787,.T.);
#7778=EDGE_CURVE('',#6215,#6213,#1219,.T.);
#7779=EDGE_CURVE('',#6212,#6214,#1220,.T.);
#7780=EDGE_CURVE('',#6216,#6180,#3788,.T.);
#7781=EDGE_CURVE('',#6180,#6215,#3789,.T.);
#7782=EDGE_CURVE('',#6214,#6216,#3790,.T.);
#7783=EDGE_CURVE('',#6195,#6209,#3791,.T.);
#7784=EDGE_CURVE('',#6199,#6211,#3792,.T.);
#7785=EDGE_CURVE('',#6197,#6213,#3793,.T.);
#7786=EDGE_CURVE('',#6183,#6215,#3794,.T.);
#7787=EDGE_CURVE('',#6216,#6217,#3795,.T.);
#7788=EDGE_CURVE('',#6217,#6181,#3796,.T.);
#7789=EDGE_CURVE('',#6218,#6119,#3797,.T.);
#7790=EDGE_CURVE('',#6119,#6181,#1221,.T.);
#7791=EDGE_CURVE('',#6217,#6218,#1222,.T.);
#7792=EDGE_CURVE('',#6218,#6219,#3798,.T.);
#7793=EDGE_CURVE('',#6219,#6113,#3799,.T.);
#7794=EDGE_CURVE('',#6219,#6220,#3800,.T.);
#7795=EDGE_CURVE('',#6220,#6108,#3801,.T.);
#7796=EDGE_CURVE('',#6220,#6221,#3802,.T.);
#7797=EDGE_CURVE('',#6221,#6109,#3803,.T.);
#7798=EDGE_CURVE('',#6222,#6131,#3804,.T.);
#7799=EDGE_CURVE('',#6131,#6109,#1223,.T.);
#7800=EDGE_CURVE('',#6221,#6222,#1224,.T.);
#7801=EDGE_CURVE('',#6222,#6223,#3805,.T.);
#7802=EDGE_CURVE('',#6223,#6128,#3806,.T.);
#7803=EDGE_CURVE('',#6223,#6224,#3807,.T.);
#7804=EDGE_CURVE('',#6224,#6129,#3808,.T.);
#7805=EDGE_CURVE('',#6225,#6226,#3809,.T.);
#7806=EDGE_CURVE('',#6226,#6129,#1225,.T.);
#7807=EDGE_CURVE('',#6224,#6225,#1226,.T.);
#7808=EDGE_CURVE('',#6227,#6228,#3810,.T.);
#7809=EDGE_CURVE('',#6228,#6226,#3811,.T.);
#7810=EDGE_CURVE('',#6225,#6227,#3812,.T.);
#7811=EDGE_CURVE('',#6229,#6139,#3813,.T.);
#7812=EDGE_CURVE('',#6139,#6228,#1227,.T.);
#7813=EDGE_CURVE('',#6227,#6229,#1228,.T.);
#7814=EDGE_CURVE('',#6229,#6230,#3814,.T.);
#7815=EDGE_CURVE('',#6230,#6140,#3815,.T.);
#7816=EDGE_CURVE('',#6230,#6231,#3816,.T.);
#7817=EDGE_CURVE('',#6231,#6232,#3817,.T.);
#7818=EDGE_CURVE('',#6232,#6140,#3818,.T.);
#7819=EDGE_CURVE('',#6233,#6234,#3819,.T.);
#7820=EDGE_CURVE('',#6234,#6232,#1229,.T.);
#7821=EDGE_CURVE('',#6231,#6233,#1230,.T.);
#7822=EDGE_CURVE('',#6155,#6234,#3820,.T.);
#7823=EDGE_CURVE('',#6233,#6235,#3821,.T.);
#7824=EDGE_CURVE('',#6235,#6155,#3822,.T.);
#7825=EDGE_CURVE('',#6235,#6236,#3823,.T.);
#7826=EDGE_CURVE('',#6236,#6156,#3824,.T.);
#7827=EDGE_CURVE('',#6236,#6237,#3825,.T.);
#7828=EDGE_CURVE('',#6237,#6238,#3826,.T.);
#7829=EDGE_CURVE('',#6238,#6156,#3827,.T.);
#7830=EDGE_CURVE('',#6239,#6201,#3828,.T.);
#7831=EDGE_CURVE('',#6201,#6238,#1231,.T.);
#7832=EDGE_CURVE('',#6237,#6239,#1232,.T.);
#7833=EDGE_CURVE('',#6239,#6207,#3829,.T.);
#7834=EDGE_CURVE('',#6240,#6240,#1233,.T.);
#7835=EDGE_CURVE('',#6241,#6170,#3830,.T.);
#7836=EDGE_CURVE('',#6241,#6241,#515,.T.);
#7837=EDGE_CURVE('',#6242,#6242,#1234,.T.);
#7838=EDGE_CURVE('',#6242,#6243,#3831,.T.);
#7839=EDGE_CURVE('',#6244,#6243,#1235,.T.);
#7840=EDGE_CURVE('',#6243,#6244,#1236,.T.);
#7841=EDGE_CURVE('',#6245,#6245,#1237,.T.);
#7842=EDGE_CURVE('',#6245,#6242,#3832,.T.);
#7843=EDGE_CURVE('',#6163,#6245,#3833,.T.);
#7844=EDGE_CURVE('',#6244,#6240,#1238,.T.);
#7845=EDGE_CURVE('',#6171,#6246,#3834,.T.);
#7846=EDGE_CURVE('',#6246,#6247,#3835,.T.);
#7847=EDGE_CURVE('',#6247,#6206,#3836,.T.);
#7848=EDGE_CURVE('',#6102,#6248,#3837,.T.);
#7849=EDGE_CURVE('',#6248,#6249,#3838,.T.);
#7850=EDGE_CURVE('',#6249,#6115,#3839,.T.);
#7851=EDGE_CURVE('',#6250,#6251,#3840,.T.);
#7852=EDGE_CURVE('',#6251,#6141,#1239,.T.);
#7853=EDGE_CURVE('',#6143,#6250,#1240,.T.);
#7854=EDGE_CURVE('',#6252,#6253,#3841,.T.);
#7855=EDGE_CURVE('',#6253,#6251,#3842,.T.);
#7856=EDGE_CURVE('',#6250,#6252,#3843,.T.);
#7857=EDGE_CURVE('',#6254,#6127,#3844,.T.);
#7858=EDGE_CURVE('',#6127,#6253,#1241,.T.);
#7859=EDGE_CURVE('',#6252,#6254,#1242,.T.);
#7860=EDGE_CURVE('',#6254,#6255,#3845,.T.);
#7861=EDGE_CURVE('',#6255,#6123,#3846,.T.);
#7862=EDGE_CURVE('',#6137,#6256,#3847,.T.);
#7863=EDGE_CURVE('',#6256,#6257,#3848,.T.);
#7864=EDGE_CURVE('',#6257,#6142,#3849,.T.);
#7865=EDGE_CURVE('',#6258,#6259,#3850,.T.);
#7866=EDGE_CURVE('',#6259,#6257,#1243,.T.);
#7867=EDGE_CURVE('',#6256,#6258,#1244,.T.);
#7868=EDGE_CURVE('',#6153,#6259,#3851,.T.);
#7869=EDGE_CURVE('',#6258,#6148,#3852,.T.);
#7870=EDGE_CURVE('',#6107,#6260,#3853,.T.);
#7871=EDGE_CURVE('',#6260,#6261,#3854,.T.);
#7872=EDGE_CURVE('',#6261,#6248,#3855,.T.);
#7873=EDGE_CURVE('',#6262,#6263,#3856,.T.);
#7874=EDGE_CURVE('',#6263,#6261,#1245,.T.);
#7875=EDGE_CURVE('',#6260,#6262,#1246,.T.);
#7876=EDGE_CURVE('',#6255,#6263,#3857,.T.);
#7877=EDGE_CURVE('',#6262,#6124,#3858,.T.);
#7878=EDGE_CURVE('',#6159,#6264,#3859,.T.);
#7879=EDGE_CURVE('',#6264,#6265,#3860,.T.);
#7880=EDGE_CURVE('',#6265,#6152,#3861,.T.);
#7881=EDGE_CURVE('',#6203,#6266,#3862,.T.);
#7882=EDGE_CURVE('',#6266,#6265,#1247,.T.);
#7883=EDGE_CURVE('',#6264,#6203,#1248,.T.);
#7884=EDGE_CURVE('',#6192,#6266,#3863,.T.);
#7885=EDGE_CURVE('',#6178,#6267,#3864,.T.);
#7886=EDGE_CURVE('',#6267,#6246,#3865,.T.);
#7887=EDGE_CURVE('',#6268,#6269,#3866,.T.);
#7888=EDGE_CURVE('',#6269,#6267,#1249,.T.);
#7889=EDGE_CURVE('',#6178,#6268,#1250,.T.);
#7890=EDGE_CURVE('',#6249,#6269,#3867,.T.);
#7891=EDGE_CURVE('',#6268,#6116,#3868,.T.);
#7892=EDGE_CURVE('',#6270,#6205,#3869,.T.);
#7893=EDGE_CURVE('',#6247,#6270,#1251,.T.);
#7894=EDGE_CURVE('',#6271,#6204,#3870,.T.);
#7895=EDGE_CURVE('',#6270,#6271,#3871,.T.);
#7896=EDGE_CURVE('',#6271,#6191,#1252,.T.);
#7897=EDGE_CURVE('',#6272,#6264,#3872,.T.);
#7898=EDGE_CURVE('',#6200,#6272,#1253,.T.);
#7899=EDGE_CURVE('',#6272,#6158,#3873,.T.);
#7900=EDGE_CURVE('',#6273,#6258,#3874,.T.);
#7901=EDGE_CURVE('',#6149,#6273,#3875,.T.);
#7902=EDGE_CURVE('',#6274,#6256,#3876,.T.);
#7903=EDGE_CURVE('',#6273,#6274,#1254,.T.);
#7904=EDGE_CURVE('',#6274,#6136,#3877,.T.);
#7905=EDGE_CURVE('',#6138,#6275,#1255,.T.);
#7906=EDGE_CURVE('',#6275,#6228,#3878,.T.);
#7907=EDGE_CURVE('',#6275,#6276,#3879,.T.);
#7908=EDGE_CURVE('',#6276,#6226,#3880,.T.);
#7909=EDGE_CURVE('',#6276,#6126,#1256,.T.);
#7910=EDGE_CURVE('',#6273,#6234,#3881,.T.);
#7911=EDGE_CURVE('',#6274,#6232,#3882,.T.);
#7912=EDGE_CURVE('',#6130,#6110,#1257,.T.);
#7913=EDGE_CURVE('',#6272,#6238,#3883,.T.);
#7914=EDGE_CURVE('',#6118,#6177,#1258,.T.);
#7915=EDGE_CURVE('',#6276,#6253,#3884,.T.);
#7916=EDGE_CURVE('',#6251,#6275,#3885,.T.);
#7917=EDGE_CURVE('',#6118,#6268,#3886,.T.);
#7918=EDGE_CURVE('',#6130,#6262,#3887,.T.);
#7919=EDGE_CURVE('',#6110,#6260,#3888,.T.);
#7920=EDGE_CURVE('',#6277,#6277,#1259,.T.);
#7921=EDGE_CURVE('',#6278,#6278,#1260,.T.);
#7922=EDGE_CURVE('',#6279,#6279,#1261,.T.);
#7923=EDGE_CURVE('',#6279,#6277,#3889,.T.);
#7924=EDGE_CURVE('',#6280,#6281,#516,.T.);
#7925=EDGE_CURVE('',#6282,#6280,#1262,.T.);
#7926=EDGE_CURVE('',#6283,#6282,#517,.T.);
#7927=EDGE_CURVE('',#6283,#6279,#3890,.T.);
#7928=EDGE_CURVE('',#6284,#6283,#518,.T.);
#7929=EDGE_CURVE('',#6285,#6284,#1263,.T.);
#7930=EDGE_CURVE('',#6281,#6285,#519,.T.);
#7931=EDGE_CURVE('',#6286,#6286,#1264,.T.);
#7932=EDGE_CURVE('',#6286,#6287,#3891,.T.);
#7933=EDGE_CURVE('',#6287,#6287,#1265,.T.);
#7934=EDGE_CURVE('',#6288,#6288,#1266,.T.);
#7935=EDGE_CURVE('',#6289,#6290,#520,.T.);
#7936=EDGE_CURVE('',#6290,#6289,#521,.T.);
#7937=EDGE_CURVE('',#6290,#6288,#3892,.T.);
#7938=EDGE_CURVE('',#6282,#6280,#3893,.T.);
#7939=EDGE_CURVE('',#6285,#6284,#3894,.T.);
#7940=EDGE_CURVE('',#6278,#6291,#3895,.T.);
#7941=EDGE_CURVE('',#6292,#6291,#522,.T.);
#7942=EDGE_CURVE('',#6293,#6292,#523,.T.);
#7943=EDGE_CURVE('',#6291,#6293,#524,.T.);
#7944=EDGE_CURVE('',#6294,#6295,#3896,.T.);
#7945=EDGE_CURVE('',#6295,#6294,#1267,.T.);
#7946=EDGE_CURVE('',#6287,#6296,#3897,.T.);
#7947=EDGE_CURVE('',#6297,#6296,#525,.T.);
#7948=EDGE_CURVE('',#6297,#6298,#1268,.T.);
#7949=EDGE_CURVE('',#6295,#6298,#526,.T.);
#7950=EDGE_CURVE('',#6296,#6294,#527,.T.);
#7951=EDGE_CURVE('',#6298,#6297,#3898,.T.);
#7952=EDGE_CURVE('',#6299,#6299,#1269,.T.);
#7953=EDGE_CURVE('',#6300,#6300,#1270,.T.);
#7954=EDGE_CURVE('',#6300,#6299,#3899,.T.);
#7955=EDGE_CURVE('',#6301,#6301,#1271,.T.);
#7956=EDGE_CURVE('',#6301,#6300,#3900,.T.);
#7957=EDGE_CURVE('',#6302,#6302,#1272,.T.);
#7958=EDGE_CURVE('',#6303,#6303,#1273,.T.);
#7959=EDGE_CURVE('',#6303,#6302,#3901,.T.);
#7960=EDGE_CURVE('',#6304,#6304,#1274,.T.);
#7961=EDGE_CURVE('',#6304,#6293,#3902,.T.);
#7962=EDGE_CURVE('',#6291,#6303,#3903,.T.);
#7963=EDGE_CURVE('',#6305,#6305,#1275,.T.);
#7964=EDGE_CURVE('',#6305,#6304,#3904,.T.);
#7965=EDGE_CURVE('',#6306,#6306,#1276,.T.);
#7966=EDGE_CURVE('',#6306,#6307,#3905,.T.);
#7967=EDGE_CURVE('',#6307,#6307,#1277,.T.);
#7968=EDGE_CURVE('',#6307,#6281,#3906,.T.);
#7969=EDGE_CURVE('',#6283,#6308,#3907,.T.);
#7970=EDGE_CURVE('',#6308,#6308,#1278,.T.);
#7971=EDGE_CURVE('',#6309,#6309,#1279,.T.);
#7972=EDGE_CURVE('',#6309,#6310,#3908,.T.);
#7973=EDGE_CURVE('',#6310,#6311,#1280,.T.);
#7974=EDGE_CURVE('',#6311,#6310,#1281,.T.);
#7975=EDGE_CURVE('',#6311,#6312,#3909,.T.);
#7976=EDGE_CURVE('',#6313,#6312,#1282,.T.);
#7977=EDGE_CURVE('',#6312,#6313,#1283,.T.);
#7978=EDGE_CURVE('',#6313,#6314,#3910,.T.);
#7979=EDGE_CURVE('',#6314,#6315,#1284,.T.);
#7980=EDGE_CURVE('',#6315,#6314,#1285,.T.);
#7981=EDGE_CURVE('',#6315,#6316,#3911,.T.);
#7982=EDGE_CURVE('',#6317,#6316,#1286,.T.);
#7983=EDGE_CURVE('',#6316,#6317,#1287,.T.);
#7984=EDGE_CURVE('',#6317,#6318,#3912,.T.);
#7985=EDGE_CURVE('',#6318,#6319,#1288,.T.);
#7986=EDGE_CURVE('',#6319,#6318,#1289,.T.);
#7987=EDGE_CURVE('',#6319,#6320,#3913,.T.);
#7988=EDGE_CURVE('',#6321,#6320,#1290,.T.);
#7989=EDGE_CURVE('',#6320,#6321,#1291,.T.);
#7990=EDGE_CURVE('',#6321,#6322,#3914,.T.);
#7991=EDGE_CURVE('',#6322,#6322,#1292,.T.);
#7992=EDGE_CURVE('',#6323,#6324,#3915,.T.);
#7993=EDGE_CURVE('',#6324,#6325,#3916,.T.);
#7994=EDGE_CURVE('',#6325,#6326,#3917,.T.);
#7995=EDGE_CURVE('',#6326,#6327,#3918,.T.);
#7996=EDGE_CURVE('',#6327,#6328,#3919,.T.);
#7997=EDGE_CURVE('',#6328,#6323,#3920,.T.);
#7998=EDGE_CURVE('',#6326,#6329,#3921,.T.);
#7999=EDGE_CURVE('',#6329,#6330,#3922,.T.);
#8000=EDGE_CURVE('',#6330,#6331,#3923,.T.);
#8001=EDGE_CURVE('',#6331,#6332,#3924,.T.);
#8002=EDGE_CURVE('',#6332,#6327,#3925,.T.);
#8003=EDGE_CURVE('',#6333,#6325,#3926,.T.);
#8004=EDGE_CURVE('',#6334,#6333,#3927,.T.);
#8005=EDGE_CURVE('',#6335,#6334,#3928,.T.);
#8006=EDGE_CURVE('',#6336,#6335,#3929,.T.);
#8007=EDGE_CURVE('',#6337,#6336,#3930,.T.);
#8008=EDGE_CURVE('',#6338,#6337,#3931,.T.);
#8009=EDGE_CURVE('',#6329,#6338,#3932,.T.);
#8010=EDGE_CURVE('',#6324,#6339,#3933,.T.);
#8011=EDGE_CURVE('',#6333,#6339,#3934,.T.);
#8012=EDGE_CURVE('',#6328,#6340,#3935,.T.);
#8013=EDGE_CURVE('',#6340,#6341,#3936,.T.);
#8014=EDGE_CURVE('',#6341,#6342,#3937,.T.);
#8015=EDGE_CURVE('',#6342,#6343,#3938,.T.);
#8016=EDGE_CURVE('',#6343,#6323,#3939,.T.);
#8017=EDGE_CURVE('',#6340,#6332,#3940,.T.);
#8018=EDGE_CURVE('',#6344,#6343,#3941,.T.);
#8019=EDGE_CURVE('',#6345,#6344,#3942,.T.);
#8020=EDGE_CURVE('',#6346,#6345,#3943,.T.);
#8021=EDGE_CURVE('',#6347,#6346,#3944,.T.);
#8022=EDGE_CURVE('',#6348,#6347,#3945,.T.);
#8023=EDGE_CURVE('',#6339,#6348,#3946,.T.);
#8024=EDGE_CURVE('',#6331,#6349,#3947,.T.);
#8025=EDGE_CURVE('',#6350,#6349,#3948,.T.);
#8026=EDGE_CURVE('',#6350,#6341,#3949,.T.);
#8027=EDGE_CURVE('',#6351,#6330,#3950,.T.);
#8028=EDGE_CURVE('',#6352,#6351,#3951,.T.);
#8029=EDGE_CURVE('',#6353,#6352,#3952,.T.);
#8030=EDGE_CURVE('',#6354,#6353,#3953,.T.);
#8031=EDGE_CURVE('',#6355,#6354,#3954,.T.);
#8032=EDGE_CURVE('',#6349,#6355,#3955,.T.);
#8033=EDGE_CURVE('',#6356,#6357,#3956,.T.);
#8034=EDGE_CURVE('',#6357,#6346,#3957,.T.);
#8035=EDGE_CURVE('',#6345,#6358,#3958,.T.);
#8036=EDGE_CURVE('',#6358,#6359,#3959,.T.);
#8037=EDGE_CURVE('',#6359,#6356,#3960,.T.);
#8038=EDGE_CURVE('',#6359,#6360,#3961,.T.);
#8039=EDGE_CURVE('',#6360,#6361,#3962,.T.);
#8040=EDGE_CURVE('',#6361,#6362,#3963,.T.);
#8041=EDGE_CURVE('',#6362,#6363,#3964,.T.);
#8042=EDGE_CURVE('',#6363,#6356,#3965,.T.);
#8043=EDGE_CURVE('',#6364,#6358,#3966,.T.);
#8044=EDGE_CURVE('',#6360,#6364,#3967,.T.);
#8045=EDGE_CURVE('',#6344,#6365,#3968,.T.);
#8046=EDGE_CURVE('',#6365,#6366,#3969,.T.);
#8047=EDGE_CURVE('',#6366,#6364,#3970,.T.);
#8048=EDGE_CURVE('',#6357,#6367,#3971,.T.);
#8049=EDGE_CURVE('',#6347,#6367,#3972,.T.);
#8050=EDGE_CURVE('',#6368,#6363,#3973,.T.);
#8051=EDGE_CURVE('',#6369,#6368,#3974,.T.);
#8052=EDGE_CURVE('',#6370,#6369,#3975,.T.);
#8053=EDGE_CURVE('',#6371,#6370,#3976,.T.);
#8054=EDGE_CURVE('',#6372,#6371,#3977,.T.);
#8055=EDGE_CURVE('',#6367,#6372,#3978,.T.);
#8056=EDGE_CURVE('',#6373,#6374,#3979,.T.);
#8057=EDGE_CURVE('',#6374,#6370,#3980,.T.);
#8058=EDGE_CURVE('',#6369,#6375,#3981,.T.);
#8059=EDGE_CURVE('',#6375,#6376,#3982,.T.);
#8060=EDGE_CURVE('',#6376,#6373,#3983,.T.);
#8061=EDGE_CURVE('',#6376,#6377,#3984,.T.);
#8062=EDGE_CURVE('',#6377,#6378,#3985,.T.);
#8063=EDGE_CURVE('',#6378,#6379,#3986,.T.);
#8064=EDGE_CURVE('',#6379,#6380,#3987,.T.);
#8065=EDGE_CURVE('',#6380,#6373,#3988,.T.);
#8066=EDGE_CURVE('',#6381,#6375,#3989,.T.);
#8067=EDGE_CURVE('',#6377,#6381,#3990,.T.);
#8068=EDGE_CURVE('',#6368,#6382,#3991,.T.);
#8069=EDGE_CURVE('',#6382,#6383,#3992,.T.);
#8070=EDGE_CURVE('',#6383,#6381,#3993,.T.);
#8071=EDGE_CURVE('',#6383,#6384,#3994,.T.);
#8072=EDGE_CURVE('',#6385,#6384,#3995,.T.);
#8073=EDGE_CURVE('',#6385,#6378,#3996,.T.);
#8074=EDGE_CURVE('',#6386,#6361,#3997,.T.);
#8075=EDGE_CURVE('',#6387,#6386,#3998,.T.);
#8076=EDGE_CURVE('',#6388,#6387,#3999,.T.);
#8077=EDGE_CURVE('',#6384,#6388,#4000,.T.);
#8078=EDGE_CURVE('',#6362,#6382,#4001,.T.);
#8079=EDGE_CURVE('',#6389,#6380,#4002,.T.);
#8080=EDGE_CURVE('',#6390,#6389,#4003,.T.);
#8081=EDGE_CURVE('',#6391,#6390,#4004,.T.);
#8082=EDGE_CURVE('',#6392,#6391,#4005,.T.);
#8083=EDGE_CURVE('',#6393,#6392,#4006,.T.);
#8084=EDGE_CURVE('',#6394,#6393,#4007,.T.);
#8085=EDGE_CURVE('',#6374,#6394,#4008,.T.);
#8086=EDGE_CURVE('',#6379,#6395,#4009,.T.);
#8087=EDGE_CURVE('',#6389,#6395,#4010,.T.);
#8088=EDGE_CURVE('',#6396,#6385,#4011,.T.);
#8089=EDGE_CURVE('',#6397,#6396,#4012,.T.);
#8090=EDGE_CURVE('',#6398,#6397,#4013,.T.);
#8091=EDGE_CURVE('',#6399,#6398,#4014,.T.);
#8092=EDGE_CURVE('',#6395,#6399,#4015,.T.);
#8093=EDGE_CURVE('',#6336,#6391,#4016,.T.);
#8094=EDGE_CURVE('',#6390,#6400,#4017,.T.);
#8095=EDGE_CURVE('',#6400,#6401,#4018,.T.);
#8096=EDGE_CURVE('',#6401,#6337,#4019,.T.);
#8097=EDGE_CURVE('',#6399,#6402,#4020,.T.);
#8098=EDGE_CURVE('',#6402,#6400,#4021,.T.);
#8099=EDGE_CURVE('',#6392,#6335,#4022,.T.);
#8100=EDGE_CURVE('',#6401,#6403,#4023,.T.);
#8101=EDGE_CURVE('',#6403,#6352,#4024,.T.);
#8102=EDGE_CURVE('',#6351,#6338,#4025,.T.);
#8103=EDGE_CURVE('',#6403,#6402,#4026,.T.);
#8104=EDGE_CURVE('',#6398,#6353,#4027,.T.);
#8105=EDGE_CURVE('',#6371,#6394,#4028,.T.);
#8106=EDGE_CURVE('',#6393,#6404,#4029,.T.);
#8107=EDGE_CURVE('',#6404,#6405,#4030,.T.);
#8108=EDGE_CURVE('',#6405,#6372,#4031,.T.);
#8109=EDGE_CURVE('',#6406,#6334,#4032,.T.);
#8110=EDGE_CURVE('',#6406,#6404,#4033,.T.);
#8111=EDGE_CURVE('',#6348,#6407,#4034,.T.);
#8112=EDGE_CURVE('',#6407,#6406,#4035,.T.);
#8113=EDGE_CURVE('',#6405,#6407,#4036,.T.);
#8114=EDGE_CURVE('',#6408,#6408,#1293,.T.);
#8115=EDGE_CURVE('',#6409,#6409,#1294,.T.);
#8116=EDGE_CURVE('',#6410,#6410,#1295,.T.);
#8117=EDGE_CURVE('',#6411,#6411,#1296,.T.);
#8118=EDGE_CURVE('',#6412,#6412,#1297,.T.);
#8119=EDGE_CURVE('',#6413,#6413,#1298,.T.);
#8120=EDGE_CURVE('',#6354,#6397,#4037,.T.);
#8121=EDGE_CURVE('',#6366,#6414,#4038,.T.);
#8122=EDGE_CURVE('',#6414,#6386,#4039,.T.);
#8123=EDGE_CURVE('',#6414,#6415,#4040,.T.);
#8124=EDGE_CURVE('',#6387,#6415,#4041,.T.);
#8125=EDGE_CURVE('',#6416,#6350,#4042,.T.);
#8126=EDGE_CURVE('',#6415,#6416,#4043,.T.);
#8127=EDGE_CURVE('',#6342,#6365,#4044,.T.);
#8128=EDGE_CURVE('',#6417,#6418,#1299,.T.);
#8129=EDGE_CURVE('',#6418,#6417,#1300,.T.);
#8130=EDGE_CURVE('',#6417,#6419,#4045,.T.);
#8131=EDGE_CURVE('',#6419,#6420,#1301,.T.);
#8132=EDGE_CURVE('',#6420,#6419,#1302,.T.);
#8133=EDGE_CURVE('',#6421,#6422,#1303,.T.);
#8134=EDGE_CURVE('',#6422,#6421,#1304,.T.);
#8135=EDGE_CURVE('',#6422,#6418,#4046,.T.);
#8136=EDGE_CURVE('',#6420,#6423,#4047,.T.);
#8137=EDGE_CURVE('',#6423,#6423,#1305,.T.);
#8138=EDGE_CURVE('',#6424,#6424,#1306,.T.);
#8139=EDGE_CURVE('',#6424,#6421,#4048,.T.);
#8140=EDGE_CURVE('',#6425,#6425,#1307,.T.);
#8141=EDGE_CURVE('',#6426,#6426,#1308,.T.);
#8142=EDGE_CURVE('',#6426,#6427,#4049,.T.);
#8143=EDGE_CURVE('',#6427,#6428,#1309,.T.);
#8144=EDGE_CURVE('',#6428,#6427,#1310,.T.);
#8145=EDGE_CURVE('',#6429,#6429,#1311,.T.);
#8146=EDGE_CURVE('',#6428,#6425,#4050,.T.);
#8147=EDGE_CURVE('',#6413,#6430,#4051,.T.);
#8148=EDGE_CURVE('',#6430,#6430,#1312,.T.);
#8149=EDGE_CURVE('',#6430,#6429,#4052,.T.);
#8150=EDGE_CURVE('',#6408,#6431,#4053,.T.);
#8151=EDGE_CURVE('',#6431,#6431,#1313,.T.);
#8152=EDGE_CURVE('',#6432,#6433,#1314,.T.);
#8153=EDGE_CURVE('',#6433,#6432,#1315,.T.);
#8154=EDGE_CURVE('',#6433,#6431,#4054,.T.);
#8155=EDGE_CURVE('',#6434,#6434,#1316,.T.);
#8156=EDGE_CURVE('',#6434,#6432,#4055,.T.);
#8157=EDGE_CURVE('',#6435,#6435,#1317,.T.);
#8158=EDGE_CURVE('',#6412,#6436,#4056,.T.);
#8159=EDGE_CURVE('',#6436,#6436,#1318,.T.);
#8160=EDGE_CURVE('',#6437,#6438,#1319,.T.);
#8161=EDGE_CURVE('',#6438,#6437,#1320,.T.);
#8162=EDGE_CURVE('',#6438,#6436,#4057,.T.);
#8163=EDGE_CURVE('',#6439,#6439,#1321,.T.);
#8164=EDGE_CURVE('',#6439,#6437,#4058,.T.);
#8165=EDGE_CURVE('',#6440,#6440,#1322,.T.);
#8166=EDGE_CURVE('',#6409,#6441,#4059,.T.);
#8167=EDGE_CURVE('',#6441,#6441,#1323,.T.);
#8168=EDGE_CURVE('',#6442,#6442,#1324,.T.);
#8169=EDGE_CURVE('',#6442,#6441,#4060,.T.);
#8170=EDGE_CURVE('',#6411,#6443,#4061,.T.);
#8171=EDGE_CURVE('',#6443,#6443,#1325,.T.);
#8172=EDGE_CURVE('',#6444,#6444,#1326,.T.);
#8173=EDGE_CURVE('',#6444,#6443,#4062,.T.);
#8174=EDGE_CURVE('',#6410,#6445,#4063,.T.);
#8175=EDGE_CURVE('',#6445,#6445,#1327,.T.);
#8176=EDGE_CURVE('',#6446,#6446,#1328,.T.);
#8177=EDGE_CURVE('',#6446,#6445,#4064,.T.);
#8178=EDGE_CURVE('',#6447,#6447,#1329,.T.);
#8179=EDGE_CURVE('',#6447,#6448,#4065,.T.);
#8180=EDGE_CURVE('',#6448,#6448,#1330,.T.);
#8181=EDGE_CURVE('',#6449,#6450,#4066,.T.);
#8182=EDGE_CURVE('',#6451,#6449,#4067,.T.);
#8183=EDGE_CURVE('',#6452,#6451,#4068,.T.);
#8184=EDGE_CURVE('',#6450,#6452,#4069,.T.);
#8185=EDGE_CURVE('',#6453,#6453,#1331,.T.);
#8186=EDGE_CURVE('',#6454,#6454,#1332,.T.);
#8187=EDGE_CURVE('',#6455,#6455,#1333,.T.);
#8188=EDGE_CURVE('',#6456,#6456,#1334,.T.);
#8189=EDGE_CURVE('',#6457,#6457,#1335,.T.);
#8190=EDGE_CURVE('',#6448,#6440,#4070,.T.);
#8191=EDGE_CURVE('',#6453,#6458,#4071,.T.);
#8192=EDGE_CURVE('',#6458,#6458,#1336,.T.);
#8193=EDGE_CURVE('',#6458,#6435,#4072,.T.);
#8194=EDGE_CURVE('',#6457,#6423,#4073,.T.);
#8195=EDGE_CURVE('',#6355,#6449,#4074,.T.);
#8196=EDGE_CURVE('',#6450,#6416,#4075,.T.);
#8197=EDGE_CURVE('',#6451,#6396,#4076,.T.);
#8198=EDGE_CURVE('',#6388,#6452,#4077,.T.);
#8199=EDGE_CURVE('',#6454,#6446,#4078,.T.);
#8200=EDGE_CURVE('',#6456,#6444,#4079,.T.);
#8201=EDGE_CURVE('',#6455,#6442,#4080,.T.);
#8202=EDGE_CURVE('',#6459,#6459,#1337,.T.);
#8203=EDGE_CURVE('',#6460,#6460,#1338,.T.);
#8204=EDGE_CURVE('',#6460,#6459,#4081,.T.);
#8205=EDGE_CURVE('',#6461,#6461,#1339,.T.);
#8206=EDGE_CURVE('',#6461,#6460,#4082,.T.);
#8207=EDGE_CURVE('',#6462,#6462,#1340,.T.);
#8208=EDGE_CURVE('',#6462,#6461,#4083,.T.);
#8209=EDGE_CURVE('',#6463,#6464,#4084,.T.);
#8210=EDGE_CURVE('',#6463,#6465,#528,.T.);
#8211=EDGE_CURVE('',#6465,#6466,#4085,.F.);
#8212=EDGE_CURVE('',#6466,#6464,#529,.T.);
#8213=EDGE_CURVE('',#6467,#6468,#4086,.T.);
#8214=EDGE_CURVE('',#6467,#6463,#530,.T.);
#8215=EDGE_CURVE('',#6464,#6468,#531,.T.);
#8216=EDGE_CURVE('',#6469,#6470,#4087,.T.);
#8217=EDGE_CURVE('',#6469,#6471,#532,.T.);
#8218=EDGE_CURVE('',#6472,#6471,#1341,.T.);
#8219=EDGE_CURVE('',#6470,#6472,#533,.T.);
#8220=EDGE_CURVE('',#6473,#6474,#4088,.T.);
#8221=EDGE_CURVE('',#6475,#6473,#1342,.T.);
#8222=EDGE_CURVE('',#6475,#6469,#534,.T.);
#8223=EDGE_CURVE('',#6474,#6470,#535,.T.);
#8224=EDGE_CURVE('',#6476,#6477,#536,.T.);
#8225=EDGE_CURVE('',#6478,#6476,#537,.T.);
#8226=EDGE_CURVE('',#6479,#6478,#538,.T.);
#8227=EDGE_CURVE('',#6479,#6474,#539,.T.);
#8228=EDGE_CURVE('',#6480,#6472,#540,.T.);
#8229=EDGE_CURVE('',#6468,#6480,#541,.T.);
#8230=EDGE_CURVE('',#6481,#6466,#542,.T.);
#8231=EDGE_CURVE('',#6482,#6481,#543,.T.);
#8232=EDGE_CURVE('',#6482,#6477,#544,.T.);
#8233=EDGE_CURVE('',#6483,#6484,#4089,.T.);
#8234=EDGE_CURVE('',#6483,#6485,#1343,.T.);
#8235=EDGE_CURVE('',#6485,#6484,#545,.T.);
#8236=EDGE_CURVE('',#6486,#6481,#4090,.T.);
#8237=EDGE_CURVE('',#6486,#6487,#1344,.T.);
#8238=EDGE_CURVE('',#6488,#6487,#4091,.T.);
#8239=EDGE_CURVE('',#6488,#6489,#546,.T.);
#8240=EDGE_CURVE('',#6489,#6482,#1345,.T.);
#8241=EDGE_CURVE('',#6490,#6491,#4092,.T.);
#8242=EDGE_CURVE('',#6490,#6492,#547,.T.);
#8243=EDGE_CURVE('',#6492,#6491,#1346,.T.);
#8244=EDGE_CURVE('',#6465,#6493,#548,.T.);
#8245=EDGE_CURVE('',#6494,#6467,#549,.T.);
#8246=EDGE_CURVE('',#6471,#6494,#550,.T.);
#8247=EDGE_CURVE('',#6493,#6475,#551,.T.);
#8248=EDGE_CURVE('',#6484,#6495,#552,.T.);
#8249=EDGE_CURVE('',#6496,#6485,#553,.T.);
#8250=EDGE_CURVE('',#6497,#6496,#554,.T.);
#8251=EDGE_CURVE('',#6495,#6497,#555,.T.);
#8252=EDGE_CURVE('',#6498,#6488,#556,.T.);
#8253=EDGE_CURVE('',#6489,#6498,#557,.T.);
#8254=EDGE_CURVE('',#6495,#6479,#4093,.T.);
#8255=EDGE_CURVE('',#6499,#6497,#4094,.T.);
#8256=EDGE_CURVE('',#6473,#6499,#1347,.T.);
#8257=EDGE_CURVE('',#6477,#6498,#4095,.T.);
#8258=EDGE_CURVE('',#6500,#6494,#1348,.F.);
#8259=EDGE_CURVE('',#6480,#6500,#1349,.F.);
#8260=EDGE_CURVE('',#6501,#6490,#558,.T.);
#8261=EDGE_CURVE('',#6492,#6501,#559,.T.);
#8262=EDGE_CURVE('',#6502,#6487,#98,.T.);
#8263=EDGE_CURVE('',#6503,#6502,#4096,.T.);
#8264=EDGE_CURVE('',#6504,#6503,#99,.T.);
#8265=EDGE_CURVE('',#6505,#6504,#4097,.T.);
#8266=EDGE_CURVE('',#6505,#6476,#4098,.T.);
#8267=EDGE_CURVE('',#6493,#6506,#4099,.T.);
#8268=EDGE_CURVE('',#6507,#6506,#4100,.T.);
#8269=EDGE_CURVE('',#6508,#6507,#100,.T.);
#8270=EDGE_CURVE('',#6509,#6508,#4101,.T.);
#8271=EDGE_CURVE('',#6486,#6509,#101,.T.);
#8272=EDGE_CURVE('',#6494,#6480,#1350,.F.);
#8273=EDGE_CURVE('',#6501,#6496,#4102,.F.);
#8274=EDGE_CURVE('',#6485,#6492,#1351,.T.);
#8275=EDGE_CURVE('',#6510,#6499,#4103,.T.);
#8276=EDGE_CURVE('',#6511,#6510,#1352,.T.);
#8277=EDGE_CURVE('',#6506,#6511,#1353,.T.);
#8278=EDGE_CURVE('',#6512,#6491,#102,.T.);
#8279=EDGE_CURVE('',#6513,#6512,#4104,.T.);
#8280=EDGE_CURVE('',#6514,#6513,#103,.T.);
#8281=EDGE_CURVE('',#6510,#6514,#4105,.T.);
#8282=EDGE_CURVE('',#6515,#6505,#1354,.T.);
#8283=EDGE_CURVE('',#6478,#6515,#4106,.T.);
#8284=EDGE_CURVE('',#6516,#6515,#4107,.T.);
#8285=EDGE_CURVE('',#6517,#6516,#104,.T.);
#8286=EDGE_CURVE('',#6518,#6517,#4108,.T.);
#8287=EDGE_CURVE('',#6483,#6518,#105,.T.);
#8288=EDGE_CURVE('',#6519,#6519,#1355,.T.);
#8289=EDGE_CURVE('',#6519,#6511,#4109,.T.);
#8290=EDGE_CURVE('',#6516,#6514,#1356,.T.);
#8291=EDGE_CURVE('',#6507,#6504,#1357,.T.);
#8292=EDGE_CURVE('',#6518,#6512,#1358,.T.);
#8293=EDGE_CURVE('',#6509,#6502,#1359,.T.);
#8294=EDGE_CURVE('',#6517,#6513,#1360,.T.);
#8295=EDGE_CURVE('',#6508,#6503,#1361,.T.);
#8296=EDGE_CURVE('',#6520,#6520,#1362,.T.);
#8297=EDGE_CURVE('',#6520,#6500,#4110,.T.);
#8298=EDGE_CURVE('',#6521,#6522,#4111,.T.);
#8299=EDGE_CURVE('',#6521,#6523,#560,.T.);
#8300=EDGE_CURVE('',#6523,#6524,#1363,.T.);
#8301=EDGE_CURVE('',#6524,#6522,#561,.T.);
#8302=EDGE_CURVE('',#6525,#6526,#4112,.T.);
#8303=EDGE_CURVE('',#6525,#6521,#562,.T.);
#8304=EDGE_CURVE('',#6522,#6526,#563,.T.);
#8305=EDGE_CURVE('',#6527,#6528,#4113,.T.);
#8306=EDGE_CURVE('',#6527,#6525,#564,.T.);
#8307=EDGE_CURVE('',#6526,#6528,#565,.T.);
#8308=EDGE_CURVE('',#6529,#6530,#4114,.T.);
#8309=EDGE_CURVE('',#6529,#6527,#566,.T.);
#8310=EDGE_CURVE('',#6528,#6530,#567,.T.);
#8311=EDGE_CURVE('',#6531,#6532,#4115,.T.);
#8312=EDGE_CURVE('',#6531,#6529,#568,.T.);
#8313=EDGE_CURVE('',#6530,#6532,#569,.T.);
#8314=EDGE_CURVE('',#6533,#6534,#4116,.T.);
#8315=EDGE_CURVE('',#6533,#6531,#570,.T.);
#8316=EDGE_CURVE('',#6532,#6534,#571,.T.);
#8317=EDGE_CURVE('',#6535,#6536,#4117,.T.);
#8318=EDGE_CURVE('',#6535,#6537,#572,.T.);
#8319=EDGE_CURVE('',#6538,#6537,#1364,.T.);
#8320=EDGE_CURVE('',#6536,#6538,#573,.T.);
#8321=EDGE_CURVE('',#6539,#6540,#4118,.T.);
#8322=EDGE_CURVE('',#6539,#6535,#574,.T.);
#8323=EDGE_CURVE('',#6540,#6536,#575,.T.);
#8324=EDGE_CURVE('',#6541,#6542,#4119,.T.);
#8325=EDGE_CURVE('',#6541,#6539,#576,.T.);
#8326=EDGE_CURVE('',#6542,#6540,#577,.T.);
#8327=EDGE_CURVE('',#6543,#6544,#4120,.T.);
#8328=EDGE_CURVE('',#6543,#6541,#578,.T.);
#8329=EDGE_CURVE('',#6544,#6542,#579,.T.);
#8330=EDGE_CURVE('',#6545,#6546,#4121,.T.);
#8331=EDGE_CURVE('',#6545,#6543,#580,.T.);
#8332=EDGE_CURVE('',#6546,#6544,#581,.T.);
#8333=EDGE_CURVE('',#6547,#6548,#4122,.T.);
#8334=EDGE_CURVE('',#6547,#6545,#582,.T.);
#8335=EDGE_CURVE('',#6548,#6546,#583,.T.);
#8336=EDGE_CURVE('',#6537,#6549,#584,.T.);
#8337=EDGE_CURVE('',#6550,#6549,#1365,.F.);
#8338=EDGE_CURVE('',#6551,#6550,#1366,.F.);
#8339=EDGE_CURVE('',#6551,#6538,#585,.T.);
#8340=EDGE_CURVE('',#6534,#6551,#586,.T.);
#8341=EDGE_CURVE('',#6552,#6524,#587,.T.);
#8342=EDGE_CURVE('',#6552,#6548,#588,.T.);
#8343=EDGE_CURVE('',#6524,#6553,#1367,.T.);
#8344=EDGE_CURVE('',#6553,#6523,#1368,.T.);
#8345=EDGE_CURVE('',#6523,#6554,#589,.T.);
#8346=EDGE_CURVE('',#6554,#6552,#1369,.T.);
#8347=EDGE_CURVE('',#6554,#6547,#590,.T.);
#8348=EDGE_CURVE('',#6549,#6533,#591,.T.);
#8349=EDGE_CURVE('',#6555,#6556,#4123,.T.);
#8350=EDGE_CURVE('',#6556,#6555,#1370,.T.);
#8351=EDGE_CURVE('',#6556,#6557,#4124,.T.);
#8352=EDGE_CURVE('',#6557,#6556,#1371,.T.);
#8353=EDGE_CURVE('',#6557,#6558,#4125,.T.);
#8354=EDGE_CURVE('',#6558,#6557,#1372,.T.);
#8355=EDGE_CURVE('',#6558,#6559,#4126,.T.);
#8356=EDGE_CURVE('',#6559,#6558,#1373,.T.);
#8357=EDGE_CURVE('',#6559,#6560,#4127,.T.);
#8358=EDGE_CURVE('',#6560,#6559,#1374,.T.);
#8359=EDGE_CURVE('',#6560,#6555,#4128,.T.);
#8360=EDGE_CURVE('',#6555,#6560,#1375,.T.);
#8361=EDGE_CURVE('',#6561,#6562,#4129,.T.);
#8362=EDGE_CURVE('',#6563,#6562,#1376,.T.);
#8363=EDGE_CURVE('',#6557,#6563,#106,.T.);
#8364=EDGE_CURVE('',#6564,#6556,#107,.T.);
#8365=EDGE_CURVE('',#6565,#6564,#1377,.T.);
#8366=EDGE_CURVE('',#6556,#6565,#108,.T.);
#8367=EDGE_CURVE('',#6566,#6555,#109,.T.);
#8368=EDGE_CURVE('',#6567,#6566,#1378,.T.);
#8369=EDGE_CURVE('',#6555,#6567,#110,.T.);
#8370=EDGE_CURVE('',#6568,#6560,#111,.T.);
#8371=EDGE_CURVE('',#6569,#6568,#1379,.T.);
#8372=EDGE_CURVE('',#6560,#6569,#112,.T.);
#8373=EDGE_CURVE('',#6570,#6559,#113,.T.);
#8374=EDGE_CURVE('',#6571,#6570,#1380,.T.);
#8375=EDGE_CURVE('',#6559,#6571,#114,.T.);
#8376=EDGE_CURVE('',#6572,#6558,#115,.T.);
#8377=EDGE_CURVE('',#6573,#6572,#1381,.T.);
#8378=EDGE_CURVE('',#6558,#6573,#116,.T.);
#8379=EDGE_CURVE('',#6574,#6557,#117,.T.);
#8380=EDGE_CURVE('',#6562,#6574,#1382,.T.);
#8381=EDGE_CURVE('',#6575,#6558,#4130,.T.);
#8382=EDGE_CURVE('',#6576,#6575,#4131,.T.);
#8383=EDGE_CURVE('',#6576,#6557,#4132,.T.);
#8384=EDGE_CURVE('',#6557,#6577,#4133,.T.);
#8385=EDGE_CURVE('',#6577,#6574,#4134,.T.);
#8386=EDGE_CURVE('',#6578,#6559,#4135,.T.);
#8387=EDGE_CURVE('',#6575,#6578,#4136,.T.);
#8388=EDGE_CURVE('',#6571,#6579,#4137,.T.);
#8389=EDGE_CURVE('',#6559,#6579,#4138,.T.);
#8390=EDGE_CURVE('',#6558,#6580,#4139,.T.);
#8391=EDGE_CURVE('',#6580,#6572,#4140,.T.);
#8392=EDGE_CURVE('',#6581,#6576,#4141,.T.);
#8393=EDGE_CURVE('',#6581,#6556,#4142,.T.);
#8394=EDGE_CURVE('',#6556,#6582,#4143,.T.);
#8395=EDGE_CURVE('',#6582,#6564,#4144,.T.);
#8396=EDGE_CURVE('',#6583,#6560,#4145,.T.);
#8397=EDGE_CURVE('',#6578,#6583,#4146,.T.);
#8398=EDGE_CURVE('',#6569,#6584,#4147,.T.);
#8399=EDGE_CURVE('',#6560,#6584,#4148,.T.);
#8400=EDGE_CURVE('',#6579,#6570,#4149,.T.);
#8401=EDGE_CURVE('',#6573,#6580,#4150,.T.);
#8402=EDGE_CURVE('',#6584,#6568,#4151,.T.);
#8403=EDGE_CURVE('',#6585,#6566,#4152,.T.);
#8404=EDGE_CURVE('',#6567,#6585,#4153,.T.);
#8405=EDGE_CURVE('',#6565,#6582,#4154,.T.);
#8406=EDGE_CURVE('',#6563,#6577,#4155,.T.);
#8407=EDGE_CURVE('',#6586,#6555,#4156,.T.);
#8408=EDGE_CURVE('',#6583,#6586,#4157,.T.);
#8409=EDGE_CURVE('',#6555,#6585,#4158,.T.);
#8410=EDGE_CURVE('',#6586,#6581,#4159,.T.);
#8411=EDGE_CURVE('',#6587,#6587,#1383,.T.);
#8412=EDGE_CURVE('',#6553,#6587,#4160,.T.);
#8413=EDGE_CURVE('',#6549,#6551,#1384,.F.);
#8414=EDGE_CURVE('',#6588,#6588,#1385,.T.);
#8415=EDGE_CURVE('',#6588,#6550,#4161,.T.);
#8416=EDGE_CURVE('',#6589,#6590,#4162,.T.);
#8417=EDGE_CURVE('',#6589,#6591,#592,.T.);
#8418=EDGE_CURVE('',#6591,#6592,#1386,.T.);
#8419=EDGE_CURVE('',#6592,#6590,#593,.T.);
#8420=EDGE_CURVE('',#6593,#6594,#4163,.T.);
#8421=EDGE_CURVE('',#6593,#6589,#594,.T.);
#8422=EDGE_CURVE('',#6590,#6594,#595,.T.);
#8423=EDGE_CURVE('',#6595,#6596,#4164,.T.);
#8424=EDGE_CURVE('',#6595,#6593,#596,.T.);
#8425=EDGE_CURVE('',#6594,#6596,#597,.T.);
#8426=EDGE_CURVE('',#6597,#6598,#4165,.T.);
#8427=EDGE_CURVE('',#6597,#6595,#598,.T.);
#8428=EDGE_CURVE('',#6596,#6598,#599,.T.);
#8429=EDGE_CURVE('',#6599,#6600,#4166,.T.);
#8430=EDGE_CURVE('',#6599,#6597,#600,.T.);
#8431=EDGE_CURVE('',#6598,#6600,#601,.T.);
#8432=EDGE_CURVE('',#6601,#6602,#4167,.T.);
#8433=EDGE_CURVE('',#6601,#6603,#602,.T.);
#8434=EDGE_CURVE('',#6602,#6603,#1387,.T.);
#8435=EDGE_CURVE('',#6604,#6605,#4168,.T.);
#8436=EDGE_CURVE('',#6604,#6601,#603,.T.);
#8437=EDGE_CURVE('',#6606,#6602,#1388,.T.);
#8438=EDGE_CURVE('',#6605,#6606,#604,.T.);
#8439=EDGE_CURVE('',#6607,#6608,#4169,.T.);
#8440=EDGE_CURVE('',#6607,#6604,#605,.T.);
#8441=EDGE_CURVE('',#6608,#6605,#606,.T.);
#8442=EDGE_CURVE('',#6609,#6610,#4170,.T.);
#8443=EDGE_CURVE('',#6609,#6607,#607,.T.);
#8444=EDGE_CURVE('',#6610,#6608,#608,.T.);
#8445=EDGE_CURVE('',#6611,#6612,#4171,.T.);
#8446=EDGE_CURVE('',#6611,#6609,#609,.T.);
#8447=EDGE_CURVE('',#6612,#6610,#610,.T.);
#8448=EDGE_CURVE('',#6603,#6613,#611,.T.);
#8449=EDGE_CURVE('',#6614,#6613,#1389,.F.);
#8450=EDGE_CURVE('',#6615,#6614,#1390,.F.);
#8451=EDGE_CURVE('',#6615,#6606,#612,.T.);
#8452=EDGE_CURVE('',#6600,#6615,#613,.T.);
#8453=EDGE_CURVE('',#6616,#6592,#614,.T.);
#8454=EDGE_CURVE('',#6616,#6612,#615,.T.);
#8455=EDGE_CURVE('',#6592,#6617,#1391,.T.);
#8456=EDGE_CURVE('',#6617,#6591,#1392,.T.);
#8457=EDGE_CURVE('',#6591,#6618,#616,.T.);
#8458=EDGE_CURVE('',#6618,#6616,#1393,.T.);
#8459=EDGE_CURVE('',#6618,#6611,#617,.T.);
#8460=EDGE_CURVE('',#6613,#6599,#618,.T.);
#8461=EDGE_CURVE('',#6619,#6620,#4172,.T.);
#8462=EDGE_CURVE('',#6620,#6619,#1394,.T.);
#8463=EDGE_CURVE('',#6620,#6621,#4173,.T.);
#8464=EDGE_CURVE('',#6621,#6620,#1395,.T.);
#8465=EDGE_CURVE('',#6621,#6622,#4174,.T.);
#8466=EDGE_CURVE('',#6622,#6621,#1396,.T.);
#8467=EDGE_CURVE('',#6622,#6623,#4175,.T.);
#8468=EDGE_CURVE('',#6623,#6622,#1397,.T.);
#8469=EDGE_CURVE('',#6623,#6624,#4176,.T.);
#8470=EDGE_CURVE('',#6624,#6623,#1398,.T.);
#8471=EDGE_CURVE('',#6624,#6619,#4177,.T.);
#8472=EDGE_CURVE('',#6619,#6624,#1399,.T.);
#8473=EDGE_CURVE('',#6625,#6626,#4178,.T.);
#8474=EDGE_CURVE('',#6627,#6626,#1400,.T.);
#8475=EDGE_CURVE('',#6621,#6627,#118,.T.);
#8476=EDGE_CURVE('',#6628,#6620,#119,.T.);
#8477=EDGE_CURVE('',#6629,#6628,#1401,.T.);
#8478=EDGE_CURVE('',#6620,#6629,#120,.T.);
#8479=EDGE_CURVE('',#6630,#6619,#121,.T.);
#8480=EDGE_CURVE('',#6631,#6630,#1402,.T.);
#8481=EDGE_CURVE('',#6619,#6631,#122,.T.);
#8482=EDGE_CURVE('',#6632,#6624,#123,.T.);
#8483=EDGE_CURVE('',#6633,#6632,#1403,.T.);
#8484=EDGE_CURVE('',#6624,#6633,#124,.T.);
#8485=EDGE_CURVE('',#6634,#6623,#125,.T.);
#8486=EDGE_CURVE('',#6635,#6634,#1404,.T.);
#8487=EDGE_CURVE('',#6623,#6635,#126,.T.);
#8488=EDGE_CURVE('',#6636,#6622,#127,.T.);
#8489=EDGE_CURVE('',#6637,#6636,#1405,.T.);
#8490=EDGE_CURVE('',#6622,#6637,#128,.T.);
#8491=EDGE_CURVE('',#6638,#6621,#129,.T.);
#8492=EDGE_CURVE('',#6626,#6638,#1406,.T.);
#8493=EDGE_CURVE('',#6639,#6622,#4179,.T.);
#8494=EDGE_CURVE('',#6640,#6639,#4180,.T.);
#8495=EDGE_CURVE('',#6640,#6621,#4181,.T.);
#8496=EDGE_CURVE('',#6621,#6641,#4182,.T.);
#8497=EDGE_CURVE('',#6641,#6638,#4183,.T.);
#8498=EDGE_CURVE('',#6642,#6623,#4184,.T.);
#8499=EDGE_CURVE('',#6639,#6642,#4185,.T.);
#8500=EDGE_CURVE('',#6635,#6643,#4186,.T.);
#8501=EDGE_CURVE('',#6623,#6643,#4187,.T.);
#8502=EDGE_CURVE('',#6622,#6644,#4188,.T.);
#8503=EDGE_CURVE('',#6644,#6636,#4189,.T.);
#8504=EDGE_CURVE('',#6645,#6640,#4190,.T.);
#8505=EDGE_CURVE('',#6645,#6620,#4191,.T.);
#8506=EDGE_CURVE('',#6620,#6646,#4192,.T.);
#8507=EDGE_CURVE('',#6646,#6628,#4193,.T.);
#8508=EDGE_CURVE('',#6647,#6624,#4194,.T.);
#8509=EDGE_CURVE('',#6642,#6647,#4195,.T.);
#8510=EDGE_CURVE('',#6633,#6648,#4196,.T.);
#8511=EDGE_CURVE('',#6624,#6648,#4197,.T.);
#8512=EDGE_CURVE('',#6643,#6634,#4198,.T.);
#8513=EDGE_CURVE('',#6637,#6644,#4199,.T.);
#8514=EDGE_CURVE('',#6648,#6632,#4200,.T.);
#8515=EDGE_CURVE('',#6649,#6630,#4201,.T.);
#8516=EDGE_CURVE('',#6631,#6649,#4202,.T.);
#8517=EDGE_CURVE('',#6629,#6646,#4203,.T.);
#8518=EDGE_CURVE('',#6627,#6641,#4204,.T.);
#8519=EDGE_CURVE('',#6650,#6619,#4205,.T.);
#8520=EDGE_CURVE('',#6647,#6650,#4206,.T.);
#8521=EDGE_CURVE('',#6619,#6649,#4207,.T.);
#8522=EDGE_CURVE('',#6650,#6645,#4208,.T.);
#8523=EDGE_CURVE('',#6651,#6651,#1407,.T.);
#8524=EDGE_CURVE('',#6617,#6651,#4209,.T.);
#8525=EDGE_CURVE('',#6613,#6615,#1408,.F.);
#8526=EDGE_CURVE('',#6652,#6652,#1409,.T.);
#8527=EDGE_CURVE('',#6652,#6614,#4210,.T.);
#8528=EDGE_CURVE('',#6653,#6654,#4211,.T.);
#8529=EDGE_CURVE('',#6654,#6655,#4212,.T.);
#8530=EDGE_CURVE('',#6655,#6656,#4213,.T.);
#8531=EDGE_CURVE('',#6656,#6657,#4214,.T.);
#8532=EDGE_CURVE('',#6657,#6658,#4215,.T.);
#8533=EDGE_CURVE('',#6658,#6653,#4216,.T.);
#8534=EDGE_CURVE('',#6659,#6656,#4217,.T.);
#8535=EDGE_CURVE('',#6659,#6660,#4218,.T.);
#8536=EDGE_CURVE('',#6661,#6660,#4219,.T.);
#8537=EDGE_CURVE('',#6661,#6657,#4220,.T.);
#8538=EDGE_CURVE('',#6655,#6662,#4221,.T.);
#8539=EDGE_CURVE('',#6662,#6663,#4222,.T.);
#8540=EDGE_CURVE('',#6663,#6659,#4223,.T.);
#8541=EDGE_CURVE('',#6664,#6654,#4224,.T.);
#8542=EDGE_CURVE('',#6665,#6664,#4225,.T.);
#8543=EDGE_CURVE('',#6655,#6665,#4226,.T.);
#8544=EDGE_CURVE('',#6666,#6667,#4227,.T.);
#8545=EDGE_CURVE('',#6667,#6668,#4228,.T.);
#8546=EDGE_CURVE('',#6668,#6669,#4229,.T.);
#8547=EDGE_CURVE('',#6669,#6666,#4230,.T.);
#8548=EDGE_CURVE('',#6667,#6670,#4231,.T.);
#8549=EDGE_CURVE('',#6670,#6671,#4232,.T.);
#8550=EDGE_CURVE('',#6671,#6668,#4233,.T.);
#8551=EDGE_CURVE('',#6669,#6672,#4234,.T.);
#8552=EDGE_CURVE('',#6672,#6673,#4235,.T.);
#8553=EDGE_CURVE('',#6673,#6666,#4236,.T.);
#8554=EDGE_CURVE('',#6674,#6673,#4237,.T.);
#8555=EDGE_CURVE('',#6674,#6675,#1410,.T.);
#8556=EDGE_CURVE('',#6675,#6676,#1411,.T.);
#8557=EDGE_CURVE('',#6670,#6676,#4238,.T.);
#8558=EDGE_CURVE('',#6677,#6678,#4239,.T.);
#8559=EDGE_CURVE('',#6678,#6679,#619,.T.);
#8560=EDGE_CURVE('',#6679,#6678,#620,.T.);
#8561=EDGE_CURVE('',#6677,#6677,#621,.T.);
#8562=EDGE_CURVE('',#6680,#6680,#1412,.T.);
#8563=EDGE_CURVE('',#6680,#6675,#4240,.T.);
#8564=EDGE_CURVE('',#6681,#6674,#96,.T.);
#8565=EDGE_CURVE('',#6682,#6681,#1413,.T.);
#8566=EDGE_CURVE('',#6676,#6682,#97,.T.);
#8567=EDGE_CURVE('',#6683,#6684,#622,.T.);
#8568=EDGE_CURVE('',#6684,#6683,#623,.T.);
#8569=EDGE_CURVE('',#6684,#6679,#4241,.T.);
#8570=EDGE_CURVE('',#6681,#6685,#130,.F.);
#8571=EDGE_CURVE('',#6685,#6686,#1414,.T.);
#8572=EDGE_CURVE('',#6682,#6686,#131,.T.);
#8573=EDGE_CURVE('',#6687,#6687,#1415,.T.);
#8574=EDGE_CURVE('',#6687,#6680,#4242,.T.);
#8575=EDGE_CURVE('',#6688,#6688,#1416,.T.);
#8576=EDGE_CURVE('',#6688,#6687,#4243,.T.);
#8577=EDGE_CURVE('',#6689,#6683,#4244,.T.);
#8578=EDGE_CURVE('',#6689,#6690,#624,.T.);
#8579=EDGE_CURVE('',#6690,#6691,#625,.T.);
#8580=EDGE_CURVE('',#6691,#6689,#626,.T.);
#8581=EDGE_CURVE('',#6692,#6692,#1417,.T.);
#8582=EDGE_CURVE('',#6692,#6693,#4245,.T.);
#8583=EDGE_CURVE('',#6693,#6693,#1418,.T.);
#8584=EDGE_CURVE('',#6688,#6694,#4246,.T.);
#8585=EDGE_CURVE('',#6694,#6694,#1419,.T.);
#8586=EDGE_CURVE('',#6695,#6695,#1420,.T.);
#8587=EDGE_CURVE('',#6696,#6697,#4247,.T.);
#8588=EDGE_CURVE('',#6697,#6698,#4248,.T.);
#8589=EDGE_CURVE('',#6698,#6699,#4249,.T.);
#8590=EDGE_CURVE('',#6699,#6696,#4250,.T.);
#8591=EDGE_CURVE('',#6700,#6701,#4251,.T.);
#8592=EDGE_CURVE('',#6701,#6665,#4252,.T.);
#8593=EDGE_CURVE('',#6664,#6700,#4253,.T.);
#8594=EDGE_CURVE('',#6697,#6665,#4254,.T.);
#8595=EDGE_CURVE('',#6701,#6698,#4255,.T.);
#8596=EDGE_CURVE('',#6664,#6696,#4256,.T.);
#8597=EDGE_CURVE('',#6699,#6700,#4257,.T.);
#8598=EDGE_CURVE('',#6702,#6654,#4258,.T.);
#8599=EDGE_CURVE('',#6703,#6702,#4259,.T.);
#8600=EDGE_CURVE('',#6703,#6696,#4260,.T.);
#8601=EDGE_CURVE('',#6704,#6705,#4261,.T.);
#8602=EDGE_CURVE('',#6705,#6706,#4262,.T.);
#8603=EDGE_CURVE('',#6706,#6707,#4263,.T.);
#8604=EDGE_CURVE('',#6707,#6708,#4264,.T.);
#8605=EDGE_CURVE('',#6708,#6709,#4265,.T.);
#8606=EDGE_CURVE('',#6709,#6704,#4266,.T.);
#8607=EDGE_CURVE('',#6704,#6710,#4267,.T.);
#8608=EDGE_CURVE('',#6710,#6711,#4268,.T.);
#8609=EDGE_CURVE('',#6711,#6712,#4269,.T.);
#8610=EDGE_CURVE('',#6712,#6713,#4270,.T.);
#8611=EDGE_CURVE('',#6713,#6705,#4271,.T.);
#8612=EDGE_CURVE('',#6709,#6714,#4272,.T.);
#8613=EDGE_CURVE('',#6715,#6714,#4273,.T.);
#8614=EDGE_CURVE('',#6716,#6715,#4274,.T.);
#8615=EDGE_CURVE('',#6710,#6716,#4275,.T.);
#8616=EDGE_CURVE('',#6717,#6708,#4276,.T.);
#8617=EDGE_CURVE('',#6714,#6717,#4277,.T.);
#8618=EDGE_CURVE('',#6662,#6718,#4278,.T.);
#8619=EDGE_CURVE('',#6718,#6719,#4279,.T.);
#8620=EDGE_CURVE('',#6719,#6663,#4280,.T.);
#8621=EDGE_CURVE('',#6706,#6719,#4281,.T.);
#8622=EDGE_CURVE('',#6720,#6718,#4282,.T.);
#8623=EDGE_CURVE('',#6720,#6721,#4283,.T.);
#8624=EDGE_CURVE('',#6722,#6721,#4284,.T.);
#8625=EDGE_CURVE('',#6722,#6707,#4285,.T.);
#8626=EDGE_CURVE('',#6671,#6720,#4286,.T.);
#8627=EDGE_CURVE('',#6662,#6723,#4287,.T.);
#8628=EDGE_CURVE('',#6723,#6668,#4288,.T.);
#8629=EDGE_CURVE('',#6697,#6723,#4289,.T.);
#8630=EDGE_CURVE('',#6724,#6725,#4290,.T.);
#8631=EDGE_CURVE('',#6725,#6726,#4291,.T.);
#8632=EDGE_CURVE('',#6726,#6702,#4292,.T.);
#8633=EDGE_CURVE('',#6702,#6724,#4293,.T.);
#8634=EDGE_CURVE('',#6653,#6727,#4294,.T.);
#8635=EDGE_CURVE('',#6727,#6724,#4295,.T.);
#8636=EDGE_CURVE('',#6725,#6728,#4296,.T.);
#8637=EDGE_CURVE('',#6729,#6728,#4297,.T.);
#8638=EDGE_CURVE('',#6729,#6730,#4298,.T.);
#8639=EDGE_CURVE('',#6731,#6730,#4299,.T.);
#8640=EDGE_CURVE('',#6731,#6732,#4300,.T.);
#8641=EDGE_CURVE('',#6726,#6732,#4301,.T.);
#8642=EDGE_CURVE('',#6733,#6727,#4302,.T.);
#8643=EDGE_CURVE('',#6734,#6733,#1421,.T.);
#8644=EDGE_CURVE('',#6735,#6734,#4303,.T.);
#8645=EDGE_CURVE('',#6728,#6735,#4304,.T.);
#8646=EDGE_CURVE('',#6658,#6736,#4305,.T.);
#8647=EDGE_CURVE('',#6736,#6733,#4306,.T.);
#8648=EDGE_CURVE('',#6735,#6715,#4307,.T.);
#8649=EDGE_CURVE('',#6717,#6729,#4308,.T.);
#8650=EDGE_CURVE('',#6737,#6734,#4309,.T.);
#8651=EDGE_CURVE('',#6737,#6738,#4310,.T.);
#8652=EDGE_CURVE('',#6738,#6716,#4311,.T.);
#8653=EDGE_CURVE('',#6739,#6740,#4312,.T.);
#8654=EDGE_CURVE('',#6740,#6741,#4313,.T.);
#8655=EDGE_CURVE('',#6741,#6742,#4314,.T.);
#8656=EDGE_CURVE('',#6742,#6739,#4315,.T.);
#8657=EDGE_CURVE('',#6743,#6744,#4316,.T.);
#8658=EDGE_CURVE('',#6744,#6745,#4317,.T.);
#8659=EDGE_CURVE('',#6745,#6746,#4318,.T.);
#8660=EDGE_CURVE('',#6746,#6743,#4319,.T.);
#8661=EDGE_CURVE('',#6747,#6748,#4320,.T.);
#8662=EDGE_CURVE('',#6748,#6745,#4321,.T.);
#8663=EDGE_CURVE('',#6744,#6739,#4322,.T.);
#8664=EDGE_CURVE('',#6742,#6747,#4323,.T.);
#8665=EDGE_CURVE('',#6740,#6743,#4324,.T.);
#8666=EDGE_CURVE('',#6746,#6749,#4325,.T.);
#8667=EDGE_CURVE('',#6749,#6750,#4326,.T.);
#8668=EDGE_CURVE('',#6750,#6741,#4327,.T.);
#8669=EDGE_CURVE('',#6751,#6749,#4328,.T.);
#8670=EDGE_CURVE('',#6750,#6751,#4329,.T.);
#8671=EDGE_CURVE('',#6752,#6748,#4330,.T.);
#8672=EDGE_CURVE('',#6752,#6751,#4331,.T.);
#8673=EDGE_CURVE('',#6712,#6737,#4332,.T.);
#8674=EDGE_CURVE('',#6738,#6711,#4333,.T.);
#8675=EDGE_CURVE('',#6753,#6753,#1422,.T.);
#8676=EDGE_CURVE('',#6754,#6754,#1423,.T.);
#8677=EDGE_CURVE('',#6755,#6755,#1424,.T.);
#8678=EDGE_CURVE('',#6756,#6756,#1425,.T.);
#8679=EDGE_CURVE('',#6753,#6757,#4334,.T.);
#8680=EDGE_CURVE('',#6757,#6757,#1426,.T.);
#8681=EDGE_CURVE('',#6758,#6757,#4335,.T.);
#8682=EDGE_CURVE('',#6756,#6759,#4336,.T.);
#8683=EDGE_CURVE('',#6759,#6759,#1427,.T.);
#8684=EDGE_CURVE('',#6759,#6760,#4337,.T.);
#8685=EDGE_CURVE('',#6760,#6760,#1428,.T.);
#8686=EDGE_CURVE('',#6754,#6761,#4338,.T.);
#8687=EDGE_CURVE('',#6761,#6761,#1429,.T.);
#8688=EDGE_CURVE('',#6761,#6762,#4339,.T.);
#8689=EDGE_CURVE('',#6762,#6762,#1430,.T.);
#8690=EDGE_CURVE('',#6736,#6737,#1431,.T.);
#8691=EDGE_CURVE('',#6712,#6661,#1432,.T.);
#8692=EDGE_CURVE('',#6660,#6713,#1433,.T.);
#8693=EDGE_CURVE('',#6763,#6763,#1434,.T.);
#8694=EDGE_CURVE('',#6763,#6755,#4340,.T.);
#8695=EDGE_CURVE('',#6763,#6764,#4341,.T.);
#8696=EDGE_CURVE('',#6764,#6764,#1435,.T.);
#8697=EDGE_CURVE('',#6765,#6765,#1436,.T.);
#8698=EDGE_CURVE('',#6765,#6760,#4342,.T.);
#8699=EDGE_CURVE('',#6766,#6767,#4343,.T.);
#8700=EDGE_CURVE('',#6768,#6766,#4344,.T.);
#8701=EDGE_CURVE('',#6769,#6768,#4345,.T.);
#8702=EDGE_CURVE('',#6767,#6769,#4346,.T.);
#8703=EDGE_CURVE('',#6770,#6770,#1437,.T.);
#8704=EDGE_CURVE('',#6771,#6771,#1438,.T.);
#8705=EDGE_CURVE('',#6770,#6762,#4347,.T.);
#8706=EDGE_CURVE('',#6730,#6722,#4348,.T.);
#8707=EDGE_CURVE('',#6722,#6769,#4349,.T.);
#8708=EDGE_CURVE('',#6768,#6730,#4350,.T.);
#8709=EDGE_CURVE('',#6767,#6721,#4351,.T.);
#8710=EDGE_CURVE('',#6721,#6731,#4352,.T.);
#8711=EDGE_CURVE('',#6731,#6766,#4353,.T.);
#8712=EDGE_CURVE('',#6686,#6685,#4354,.T.);
#8713=EDGE_CURVE('',#6732,#6672,#4355,.T.);
#8714=EDGE_CURVE('',#6764,#6772,#4356,.T.);
#8715=EDGE_CURVE('',#6772,#6772,#1439,.T.);
#8716=EDGE_CURVE('',#6773,#6773,#1440,.T.);
#8717=EDGE_CURVE('',#6773,#6772,#4357,.T.);
#8718=EDGE_CURVE('',#6774,#6774,#1441,.T.);
#8719=EDGE_CURVE('',#6774,#6771,#4358,.T.);
#8720=EDGE_CURVE('',#6774,#6775,#4359,.T.);
#8721=EDGE_CURVE('',#6775,#6775,#1442,.T.);
#8722=EDGE_CURVE('',#6775,#6773,#4360,.T.);
#8723=EDGE_CURVE('',#6747,#6752,#4361,.T.);
#8724=EDGE_CURVE('',#6695,#6692,#4362,.T.);
#8725=EDGE_CURVE('',#6669,#6703,#4363,.T.);
#8726=EDGE_CURVE('',#6736,#6661,#4364,.T.);
#8727=EDGE_CURVE('',#6776,#6777,#4365,.T.);
#8728=EDGE_CURVE('',#6776,#6778,#627,.T.);
#8729=EDGE_CURVE('',#6778,#6779,#1443,.T.);
#8730=EDGE_CURVE('',#6779,#6777,#628,.T.);
#8731=EDGE_CURVE('',#6780,#6781,#4366,.T.);
#8732=EDGE_CURVE('',#6780,#6776,#629,.T.);
#8733=EDGE_CURVE('',#6777,#6781,#630,.T.);
#8734=EDGE_CURVE('',#6782,#6783,#4367,.T.);
#8735=EDGE_CURVE('',#6782,#6780,#631,.T.);
#8736=EDGE_CURVE('',#6781,#6783,#632,.T.);
#8737=EDGE_CURVE('',#6784,#6785,#4368,.T.);
#8738=EDGE_CURVE('',#6784,#6782,#633,.T.);
#8739=EDGE_CURVE('',#6783,#6785,#634,.T.);
#8740=EDGE_CURVE('',#6786,#6787,#4369,.T.);
#8741=EDGE_CURVE('',#6786,#6784,#635,.T.);
#8742=EDGE_CURVE('',#6785,#6787,#636,.T.);
#8743=EDGE_CURVE('',#6788,#6789,#4370,.T.);
#8744=EDGE_CURVE('',#6788,#6786,#637,.T.);
#8745=EDGE_CURVE('',#6787,#6789,#638,.T.);
#8746=EDGE_CURVE('',#6790,#6791,#4371,.T.);
#8747=EDGE_CURVE('',#6790,#6788,#639,.T.);
#8748=EDGE_CURVE('',#6789,#6791,#640,.T.);
#8749=EDGE_CURVE('',#6792,#6793,#4372,.T.);
#8750=EDGE_CURVE('',#6792,#6790,#641,.T.);
#8751=EDGE_CURVE('',#6791,#6793,#642,.T.);
#8752=EDGE_CURVE('',#6794,#6795,#4373,.T.);
#8753=EDGE_CURVE('',#6794,#6792,#643,.T.);
#8754=EDGE_CURVE('',#6793,#6795,#644,.T.);
#8755=EDGE_CURVE('',#6796,#6797,#4374,.T.);
#8756=EDGE_CURVE('',#6796,#6794,#645,.T.);
#8757=EDGE_CURVE('',#6795,#6797,#646,.T.);
#8758=EDGE_CURVE('',#6798,#6799,#4375,.T.);
#8759=EDGE_CURVE('',#6798,#6796,#647,.T.);
#8760=EDGE_CURVE('',#6797,#6799,#648,.T.);
#8761=EDGE_CURVE('',#6800,#6801,#4376,.T.);
#8762=EDGE_CURVE('',#6800,#6798,#649,.T.);
#8763=EDGE_CURVE('',#6799,#6801,#650,.T.);
#8764=EDGE_CURVE('',#6802,#6803,#4377,.T.);
#8765=EDGE_CURVE('',#6802,#6800,#651,.T.);
#8766=EDGE_CURVE('',#6801,#6803,#652,.T.);
#8767=EDGE_CURVE('',#6804,#6805,#4378,.T.);
#8768=EDGE_CURVE('',#6804,#6802,#653,.T.);
#8769=EDGE_CURVE('',#6803,#6805,#654,.T.);
#8770=EDGE_CURVE('',#6806,#6807,#4379,.T.);
#8771=EDGE_CURVE('',#6806,#6804,#655,.T.);
#8772=EDGE_CURVE('',#6805,#6807,#656,.T.);
#8773=EDGE_CURVE('',#6808,#6809,#4380,.T.);
#8774=EDGE_CURVE('',#6808,#6806,#657,.T.);
#8775=EDGE_CURVE('',#6807,#6809,#658,.T.);
#8776=EDGE_CURVE('',#6810,#6811,#4381,.T.);
#8777=EDGE_CURVE('',#6810,#6808,#659,.T.);
#8778=EDGE_CURVE('',#6809,#6811,#660,.T.);
#8779=EDGE_CURVE('',#6812,#6813,#4382,.T.);
#8780=EDGE_CURVE('',#6812,#6810,#661,.T.);
#8781=EDGE_CURVE('',#6811,#6813,#662,.T.);
#8782=EDGE_CURVE('',#6814,#6815,#4383,.T.);
#8783=EDGE_CURVE('',#6814,#6812,#663,.T.);
#8784=EDGE_CURVE('',#6813,#6815,#664,.T.);
#8785=EDGE_CURVE('',#6816,#6817,#4384,.T.);
#8786=EDGE_CURVE('',#6816,#6814,#665,.T.);
#8787=EDGE_CURVE('',#6815,#6817,#666,.T.);
#8788=EDGE_CURVE('',#6818,#6819,#4385,.T.);
#8789=EDGE_CURVE('',#6818,#6816,#667,.T.);
#8790=EDGE_CURVE('',#6817,#6819,#668,.T.);
#8791=EDGE_CURVE('',#6820,#6821,#4386,.T.);
#8792=EDGE_CURVE('',#6820,#6818,#669,.T.);
#8793=EDGE_CURVE('',#6819,#6821,#670,.T.);
#8794=EDGE_CURVE('',#6822,#6823,#4387,.T.);
#8795=EDGE_CURVE('',#6822,#6820,#671,.T.);
#8796=EDGE_CURVE('',#6821,#6823,#672,.T.);
#8797=EDGE_CURVE('',#6824,#6825,#4388,.T.);
#8798=EDGE_CURVE('',#6826,#6824,#1444,.T.);
#8799=EDGE_CURVE('',#6826,#6822,#673,.T.);
#8800=EDGE_CURVE('',#6823,#6825,#674,.T.);
#8801=EDGE_CURVE('',#6827,#6828,#4389,.T.);
#8802=EDGE_CURVE('',#6827,#6829,#675,.T.);
#8803=EDGE_CURVE('',#6830,#6829,#1445,.T.);
#8804=EDGE_CURVE('',#6828,#6830,#676,.T.);
#8805=EDGE_CURVE('',#6831,#6832,#4390,.T.);
#8806=EDGE_CURVE('',#6831,#6827,#677,.T.);
#8807=EDGE_CURVE('',#6832,#6828,#678,.T.);
#8808=EDGE_CURVE('',#6833,#6834,#4391,.T.);
#8809=EDGE_CURVE('',#6833,#6831,#679,.T.);
#8810=EDGE_CURVE('',#6834,#6832,#680,.T.);
#8811=EDGE_CURVE('',#6835,#6836,#4392,.T.);
#8812=EDGE_CURVE('',#6835,#6833,#681,.T.);
#8813=EDGE_CURVE('',#6836,#6834,#682,.T.);
#8814=EDGE_CURVE('',#6837,#6838,#4393,.T.);
#8815=EDGE_CURVE('',#6837,#6835,#683,.T.);
#8816=EDGE_CURVE('',#6838,#6836,#684,.T.);
#8817=EDGE_CURVE('',#6839,#6840,#4394,.T.);
#8818=EDGE_CURVE('',#6839,#6837,#685,.T.);
#8819=EDGE_CURVE('',#6840,#6838,#686,.T.);
#8820=EDGE_CURVE('',#6841,#6842,#4395,.T.);
#8821=EDGE_CURVE('',#6841,#6839,#687,.T.);
#8822=EDGE_CURVE('',#6842,#6840,#688,.T.);
#8823=EDGE_CURVE('',#6843,#6844,#4396,.T.);
#8824=EDGE_CURVE('',#6843,#6841,#689,.T.);
#8825=EDGE_CURVE('',#6844,#6842,#690,.T.);
#8826=EDGE_CURVE('',#6845,#6846,#4397,.T.);
#8827=EDGE_CURVE('',#6845,#6843,#691,.T.);
#8828=EDGE_CURVE('',#6846,#6844,#692,.T.);
#8829=EDGE_CURVE('',#6847,#6848,#4398,.T.);
#8830=EDGE_CURVE('',#6847,#6845,#693,.T.);
#8831=EDGE_CURVE('',#6848,#6846,#694,.T.);
#8832=EDGE_CURVE('',#6849,#6850,#4399,.T.);
#8833=EDGE_CURVE('',#6849,#6847,#695,.T.);
#8834=EDGE_CURVE('',#6850,#6848,#696,.T.);
#8835=EDGE_CURVE('',#6851,#6852,#4400,.T.);
#8836=EDGE_CURVE('',#6851,#6849,#697,.T.);
#8837=EDGE_CURVE('',#6852,#6850,#698,.T.);
#8838=EDGE_CURVE('',#6853,#6854,#4401,.T.);
#8839=EDGE_CURVE('',#6853,#6851,#699,.T.);
#8840=EDGE_CURVE('',#6854,#6852,#700,.T.);
#8841=EDGE_CURVE('',#6855,#6856,#4402,.T.);
#8842=EDGE_CURVE('',#6855,#6853,#701,.T.);
#8843=EDGE_CURVE('',#6856,#6854,#702,.T.);
#8844=EDGE_CURVE('',#6857,#6858,#4403,.T.);
#8845=EDGE_CURVE('',#6857,#6855,#703,.T.);
#8846=EDGE_CURVE('',#6858,#6856,#704,.T.);
#8847=EDGE_CURVE('',#6859,#6860,#4404,.T.);
#8848=EDGE_CURVE('',#6859,#6857,#705,.T.);
#8849=EDGE_CURVE('',#6860,#6858,#706,.T.);
#8850=EDGE_CURVE('',#6861,#6862,#4405,.T.);
#8851=EDGE_CURVE('',#6861,#6859,#707,.T.);
#8852=EDGE_CURVE('',#6862,#6860,#708,.T.);
#8853=EDGE_CURVE('',#6863,#6864,#4406,.T.);
#8854=EDGE_CURVE('',#6863,#6861,#709,.T.);
#8855=EDGE_CURVE('',#6864,#6862,#710,.T.);
#8856=EDGE_CURVE('',#6865,#6866,#4407,.T.);
#8857=EDGE_CURVE('',#6865,#6863,#711,.T.);
#8858=EDGE_CURVE('',#6866,#6864,#712,.T.);
#8859=EDGE_CURVE('',#6867,#6868,#4408,.T.);
#8860=EDGE_CURVE('',#6867,#6865,#713,.T.);
#8861=EDGE_CURVE('',#6868,#6866,#714,.T.);
#8862=EDGE_CURVE('',#6869,#6870,#4409,.T.);
#8863=EDGE_CURVE('',#6869,#6867,#715,.T.);
#8864=EDGE_CURVE('',#6870,#6868,#716,.T.);
#8865=EDGE_CURVE('',#6871,#6872,#4410,.T.);
#8866=EDGE_CURVE('',#6871,#6869,#717,.T.);
#8867=EDGE_CURVE('',#6872,#6870,#718,.T.);
#8868=EDGE_CURVE('',#6873,#6874,#4411,.T.);
#8869=EDGE_CURVE('',#6873,#6871,#719,.T.);
#8870=EDGE_CURVE('',#6874,#6872,#720,.T.);
#8871=EDGE_CURVE('',#6875,#6876,#4412,.T.);
#8872=EDGE_CURVE('',#6875,#6877,#4413,.T.);
#8873=EDGE_CURVE('',#6877,#6878,#4414,.T.);
#8874=EDGE_CURVE('',#6876,#6878,#4415,.T.);
#8875=EDGE_CURVE('',#6879,#6875,#4416,.T.);
#8876=EDGE_CURVE('',#6879,#6880,#4417,.T.);
#8877=EDGE_CURVE('',#6880,#6877,#4418,.T.);
#8878=EDGE_CURVE('',#6881,#6879,#4419,.T.);
#8879=EDGE_CURVE('',#6881,#6882,#4420,.T.);
#8880=EDGE_CURVE('',#6882,#6880,#4421,.T.);
#8881=EDGE_CURVE('',#6876,#6881,#4422,.T.);
#8882=EDGE_CURVE('',#6878,#6882,#4423,.T.);
#8883=EDGE_CURVE('',#6883,#6883,#1446,.T.);
#8884=EDGE_CURVE('',#6883,#6884,#4424,.T.);
#8885=EDGE_CURVE('',#6884,#6884,#1447,.T.);
#8886=EDGE_CURVE('',#6885,#6830,#721,.T.);
#8887=EDGE_CURVE('',#6825,#6885,#722,.T.);
#8888=EDGE_CURVE('',#6886,#6779,#723,.T.);
#8889=EDGE_CURVE('',#6886,#6874,#724,.T.);
#8890=EDGE_CURVE('',#6779,#6887,#1448,.T.);
#8891=EDGE_CURVE('',#6887,#6778,#1449,.T.);
#8892=EDGE_CURVE('',#6778,#6888,#725,.T.);
#8893=EDGE_CURVE('',#6888,#6886,#1450,.T.);
#8894=EDGE_CURVE('',#6888,#6873,#726,.T.);
#8895=EDGE_CURVE('',#6829,#6826,#727,.T.);
#8896=EDGE_CURVE('',#6889,#6890,#132,.T.);
#8897=EDGE_CURVE('',#6889,#6891,#4425,.T.);
#8898=EDGE_CURVE('',#6892,#6891,#133,.T.);
#8899=EDGE_CURVE('',#6890,#6892,#4426,.T.);
#8900=EDGE_CURVE('',#6893,#6889,#134,.T.);
#8901=EDGE_CURVE('',#6894,#6893,#4427,.T.);
#8902=EDGE_CURVE('',#6891,#6894,#135,.T.);
#8903=EDGE_CURVE('',#6895,#6896,#136,.T.);
#8904=EDGE_CURVE('',#6895,#6897,#4428,.T.);
#8905=EDGE_CURVE('',#6898,#6897,#137,.T.);
#8906=EDGE_CURVE('',#6896,#6898,#4429,.T.);
#8907=EDGE_CURVE('',#6899,#6895,#138,.T.);
#8908=EDGE_CURVE('',#6900,#6899,#4430,.T.);
#8909=EDGE_CURVE('',#6897,#6900,#139,.T.);
#8910=EDGE_CURVE('',#6901,#6902,#140,.T.);
#8911=EDGE_CURVE('',#6901,#6903,#4431,.T.);
#8912=EDGE_CURVE('',#6904,#6903,#141,.T.);
#8913=EDGE_CURVE('',#6902,#6904,#4432,.T.);
#8914=EDGE_CURVE('',#6905,#6901,#142,.T.);
#8915=EDGE_CURVE('',#6906,#6905,#4433,.T.);
#8916=EDGE_CURVE('',#6903,#6906,#143,.T.);
#8917=EDGE_CURVE('',#6907,#6908,#144,.T.);
#8918=EDGE_CURVE('',#6907,#6909,#4434,.T.);
#8919=EDGE_CURVE('',#6910,#6909,#145,.T.);
#8920=EDGE_CURVE('',#6908,#6910,#4435,.T.);
#8921=EDGE_CURVE('',#6911,#6907,#146,.T.);
#8922=EDGE_CURVE('',#6912,#6911,#4436,.T.);
#8923=EDGE_CURVE('',#6909,#6912,#147,.T.);
#8924=EDGE_CURVE('',#6913,#6914,#148,.T.);
#8925=EDGE_CURVE('',#6913,#6915,#4437,.T.);
#8926=EDGE_CURVE('',#6916,#6915,#149,.T.);
#8927=EDGE_CURVE('',#6914,#6916,#4438,.T.);
#8928=EDGE_CURVE('',#6917,#6913,#150,.T.);
#8929=EDGE_CURVE('',#6918,#6917,#4439,.T.);
#8930=EDGE_CURVE('',#6915,#6918,#151,.T.);
#8931=EDGE_CURVE('',#6919,#6920,#152,.T.);
#8932=EDGE_CURVE('',#6919,#6921,#4440,.T.);
#8933=EDGE_CURVE('',#6922,#6921,#153,.T.);
#8934=EDGE_CURVE('',#6920,#6922,#4441,.T.);
#8935=EDGE_CURVE('',#6923,#6919,#154,.T.);
#8936=EDGE_CURVE('',#6924,#6923,#4442,.T.);
#8937=EDGE_CURVE('',#6921,#6924,#155,.T.);
#8938=EDGE_CURVE('',#6925,#6926,#156,.T.);
#8939=EDGE_CURVE('',#6925,#6927,#4443,.T.);
#8940=EDGE_CURVE('',#6928,#6927,#157,.T.);
#8941=EDGE_CURVE('',#6926,#6928,#4444,.T.);
#8942=EDGE_CURVE('',#6929,#6925,#158,.T.);
#8943=EDGE_CURVE('',#6930,#6929,#4445,.T.);
#8944=EDGE_CURVE('',#6927,#6930,#159,.T.);
#8945=EDGE_CURVE('',#6931,#6932,#160,.T.);
#8946=EDGE_CURVE('',#6931,#6933,#4446,.T.);
#8947=EDGE_CURVE('',#6934,#6933,#161,.T.);
#8948=EDGE_CURVE('',#6932,#6934,#4447,.T.);
#8949=EDGE_CURVE('',#6935,#6931,#162,.T.);
#8950=EDGE_CURVE('',#6936,#6935,#4448,.T.);
#8951=EDGE_CURVE('',#6933,#6936,#163,.T.);
#8952=EDGE_CURVE('',#6937,#6938,#164,.T.);
#8953=EDGE_CURVE('',#6937,#6939,#4449,.T.);
#8954=EDGE_CURVE('',#6940,#6939,#165,.T.);
#8955=EDGE_CURVE('',#6938,#6940,#4450,.T.);
#8956=EDGE_CURVE('',#6941,#6937,#166,.T.);
#8957=EDGE_CURVE('',#6942,#6941,#4451,.T.);
#8958=EDGE_CURVE('',#6939,#6942,#167,.T.);
#8959=EDGE_CURVE('',#6943,#6944,#168,.T.);
#8960=EDGE_CURVE('',#6943,#6945,#4452,.T.);
#8961=EDGE_CURVE('',#6946,#6945,#169,.T.);
#8962=EDGE_CURVE('',#6944,#6946,#4453,.T.);
#8963=EDGE_CURVE('',#6947,#6943,#170,.T.);
#8964=EDGE_CURVE('',#6948,#6947,#4454,.T.);
#8965=EDGE_CURVE('',#6945,#6948,#171,.T.);
#8966=EDGE_CURVE('',#6949,#6950,#172,.T.);
#8967=EDGE_CURVE('',#6949,#6951,#4455,.T.);
#8968=EDGE_CURVE('',#6952,#6951,#173,.T.);
#8969=EDGE_CURVE('',#6950,#6952,#4456,.T.);
#8970=EDGE_CURVE('',#6953,#6949,#174,.T.);
#8971=EDGE_CURVE('',#6954,#6953,#4457,.T.);
#8972=EDGE_CURVE('',#6951,#6954,#175,.T.);
#8973=EDGE_CURVE('',#6955,#6956,#176,.T.);
#8974=EDGE_CURVE('',#6955,#6957,#4458,.T.);
#8975=EDGE_CURVE('',#6958,#6957,#177,.T.);
#8976=EDGE_CURVE('',#6956,#6958,#4459,.T.);
#8977=EDGE_CURVE('',#6959,#6955,#178,.T.);
#8978=EDGE_CURVE('',#6960,#6959,#4460,.T.);
#8979=EDGE_CURVE('',#6957,#6960,#179,.T.);
#8980=EDGE_CURVE('',#6961,#6962,#180,.T.);
#8981=EDGE_CURVE('',#6961,#6963,#4461,.T.);
#8982=EDGE_CURVE('',#6964,#6963,#181,.T.);
#8983=EDGE_CURVE('',#6962,#6964,#4462,.T.);
#8984=EDGE_CURVE('',#6965,#6961,#182,.T.);
#8985=EDGE_CURVE('',#6966,#6965,#4463,.T.);
#8986=EDGE_CURVE('',#6963,#6966,#183,.T.);
#8987=EDGE_CURVE('',#6967,#6968,#184,.T.);
#8988=EDGE_CURVE('',#6967,#6969,#4464,.T.);
#8989=EDGE_CURVE('',#6970,#6969,#185,.T.);
#8990=EDGE_CURVE('',#6968,#6970,#4465,.T.);
#8991=EDGE_CURVE('',#6971,#6967,#186,.T.);
#8992=EDGE_CURVE('',#6972,#6971,#4466,.T.);
#8993=EDGE_CURVE('',#6969,#6972,#187,.T.);
#8994=EDGE_CURVE('',#6973,#6974,#188,.T.);
#8995=EDGE_CURVE('',#6973,#6975,#4467,.T.);
#8996=EDGE_CURVE('',#6976,#6975,#189,.T.);
#8997=EDGE_CURVE('',#6974,#6976,#4468,.T.);
#8998=EDGE_CURVE('',#6977,#6973,#190,.T.);
#8999=EDGE_CURVE('',#6978,#6977,#4469,.T.);
#9000=EDGE_CURVE('',#6975,#6978,#191,.T.);
#9001=EDGE_CURVE('',#6979,#6980,#192,.T.);
#9002=EDGE_CURVE('',#6979,#6981,#4470,.T.);
#9003=EDGE_CURVE('',#6982,#6981,#193,.T.);
#9004=EDGE_CURVE('',#6980,#6982,#4471,.T.);
#9005=EDGE_CURVE('',#6983,#6979,#194,.T.);
#9006=EDGE_CURVE('',#6984,#6983,#4472,.T.);
#9007=EDGE_CURVE('',#6981,#6984,#195,.T.);
#9008=EDGE_CURVE('',#6985,#6986,#196,.T.);
#9009=EDGE_CURVE('',#6985,#6987,#4473,.T.);
#9010=EDGE_CURVE('',#6988,#6987,#197,.T.);
#9011=EDGE_CURVE('',#6986,#6988,#4474,.T.);
#9012=EDGE_CURVE('',#6989,#6985,#198,.T.);
#9013=EDGE_CURVE('',#6990,#6989,#4475,.T.);
#9014=EDGE_CURVE('',#6987,#6990,#199,.T.);
#9015=EDGE_CURVE('',#6991,#6992,#200,.T.);
#9016=EDGE_CURVE('',#6991,#6993,#4476,.T.);
#9017=EDGE_CURVE('',#6994,#6993,#201,.T.);
#9018=EDGE_CURVE('',#6992,#6994,#4477,.T.);
#9019=EDGE_CURVE('',#6995,#6991,#202,.T.);
#9020=EDGE_CURVE('',#6996,#6995,#4478,.T.);
#9021=EDGE_CURVE('',#6993,#6996,#203,.T.);
#9022=EDGE_CURVE('',#6997,#6998,#204,.T.);
#9023=EDGE_CURVE('',#6997,#6999,#4479,.T.);
#9024=EDGE_CURVE('',#7000,#6999,#205,.T.);
#9025=EDGE_CURVE('',#6998,#7000,#4480,.T.);
#9026=EDGE_CURVE('',#7001,#6997,#206,.T.);
#9027=EDGE_CURVE('',#7002,#7001,#4481,.T.);
#9028=EDGE_CURVE('',#6999,#7002,#207,.T.);
#9029=EDGE_CURVE('',#7003,#7004,#208,.T.);
#9030=EDGE_CURVE('',#7003,#7005,#4482,.T.);
#9031=EDGE_CURVE('',#7006,#7005,#209,.T.);
#9032=EDGE_CURVE('',#7004,#7006,#4483,.T.);
#9033=EDGE_CURVE('',#7007,#7003,#210,.T.);
#9034=EDGE_CURVE('',#7008,#7007,#4484,.T.);
#9035=EDGE_CURVE('',#7005,#7008,#211,.T.);
#9036=EDGE_CURVE('',#7009,#7010,#212,.T.);
#9037=EDGE_CURVE('',#7009,#7011,#4485,.T.);
#9038=EDGE_CURVE('',#7012,#7011,#213,.T.);
#9039=EDGE_CURVE('',#7010,#7012,#4486,.T.);
#9040=EDGE_CURVE('',#7013,#7009,#214,.T.);
#9041=EDGE_CURVE('',#7014,#7013,#4487,.T.);
#9042=EDGE_CURVE('',#7011,#7014,#215,.T.);
#9043=EDGE_CURVE('',#7015,#7016,#216,.T.);
#9044=EDGE_CURVE('',#7015,#7017,#4488,.T.);
#9045=EDGE_CURVE('',#7018,#7017,#217,.T.);
#9046=EDGE_CURVE('',#7016,#7018,#4489,.T.);
#9047=EDGE_CURVE('',#7019,#7015,#218,.T.);
#9048=EDGE_CURVE('',#7020,#7019,#4490,.T.);
#9049=EDGE_CURVE('',#7017,#7020,#219,.T.);
#9050=EDGE_CURVE('',#7021,#7022,#220,.T.);
#9051=EDGE_CURVE('',#7021,#7023,#4491,.T.);
#9052=EDGE_CURVE('',#7024,#7023,#221,.T.);
#9053=EDGE_CURVE('',#7022,#7024,#4492,.T.);
#9054=EDGE_CURVE('',#7025,#7021,#222,.T.);
#9055=EDGE_CURVE('',#7026,#7025,#4493,.T.);
#9056=EDGE_CURVE('',#7023,#7026,#223,.T.);
#9057=EDGE_CURVE('',#7027,#7028,#224,.T.);
#9058=EDGE_CURVE('',#7027,#7029,#4494,.T.);
#9059=EDGE_CURVE('',#7030,#7029,#225,.T.);
#9060=EDGE_CURVE('',#7028,#7030,#4495,.T.);
#9061=EDGE_CURVE('',#7031,#7027,#226,.T.);
#9062=EDGE_CURVE('',#7032,#7031,#4496,.T.);
#9063=EDGE_CURVE('',#7029,#7032,#227,.T.);
#9064=EDGE_CURVE('',#7033,#7034,#228,.T.);
#9065=EDGE_CURVE('',#7033,#7035,#4497,.T.);
#9066=EDGE_CURVE('',#7036,#7035,#229,.T.);
#9067=EDGE_CURVE('',#7034,#7036,#4498,.T.);
#9068=EDGE_CURVE('',#7037,#7033,#230,.T.);
#9069=EDGE_CURVE('',#7038,#7037,#4499,.T.);
#9070=EDGE_CURVE('',#7035,#7038,#231,.T.);
#9071=EDGE_CURVE('',#7039,#7040,#232,.T.);
#9072=EDGE_CURVE('',#7039,#7041,#4500,.T.);
#9073=EDGE_CURVE('',#7042,#7041,#233,.T.);
#9074=EDGE_CURVE('',#7040,#7042,#4501,.T.);
#9075=EDGE_CURVE('',#7043,#7039,#234,.T.);
#9076=EDGE_CURVE('',#7044,#7043,#4502,.T.);
#9077=EDGE_CURVE('',#7041,#7044,#235,.T.);
#9078=EDGE_CURVE('',#7045,#7046,#236,.T.);
#9079=EDGE_CURVE('',#7045,#7047,#4503,.T.);
#9080=EDGE_CURVE('',#7048,#7047,#237,.T.);
#9081=EDGE_CURVE('',#7046,#7048,#4504,.T.);
#9082=EDGE_CURVE('',#7049,#7045,#238,.T.);
#9083=EDGE_CURVE('',#7050,#7049,#4505,.T.);
#9084=EDGE_CURVE('',#7047,#7050,#239,.T.);
#9085=EDGE_CURVE('',#7051,#7052,#240,.T.);
#9086=EDGE_CURVE('',#7051,#7053,#4506,.T.);
#9087=EDGE_CURVE('',#7054,#7053,#241,.T.);
#9088=EDGE_CURVE('',#7052,#7054,#4507,.T.);
#9089=EDGE_CURVE('',#7055,#7051,#242,.T.);
#9090=EDGE_CURVE('',#7056,#7055,#4508,.T.);
#9091=EDGE_CURVE('',#7053,#7056,#243,.T.);
#9092=EDGE_CURVE('',#7057,#7058,#244,.T.);
#9093=EDGE_CURVE('',#7057,#7059,#4509,.T.);
#9094=EDGE_CURVE('',#7060,#7059,#245,.T.);
#9095=EDGE_CURVE('',#7058,#7060,#4510,.T.);
#9096=EDGE_CURVE('',#7061,#7057,#246,.T.);
#9097=EDGE_CURVE('',#7062,#7061,#4511,.T.);
#9098=EDGE_CURVE('',#7059,#7062,#247,.T.);
#9099=EDGE_CURVE('',#7063,#7064,#248,.T.);
#9100=EDGE_CURVE('',#7063,#7065,#4512,.T.);
#9101=EDGE_CURVE('',#7066,#7065,#249,.T.);
#9102=EDGE_CURVE('',#7064,#7066,#4513,.T.);
#9103=EDGE_CURVE('',#7067,#7063,#250,.T.);
#9104=EDGE_CURVE('',#7068,#7067,#4514,.T.);
#9105=EDGE_CURVE('',#7065,#7068,#251,.T.);
#9106=EDGE_CURVE('',#7018,#7026,#1451,.T.);
#9107=EDGE_CURVE('',#7016,#7025,#1452,.T.);
#9108=EDGE_CURVE('',#6976,#6984,#1453,.T.);
#9109=EDGE_CURVE('',#6974,#6983,#1454,.T.);
#9110=EDGE_CURVE('',#6980,#6971,#1455,.T.);
#9111=EDGE_CURVE('',#6982,#6972,#1456,.T.);
#9112=EDGE_CURVE('',#6970,#6990,#1457,.T.);
#9113=EDGE_CURVE('',#6968,#6989,#1458,.T.);
#9114=EDGE_CURVE('',#6986,#6965,#1459,.T.);
#9115=EDGE_CURVE('',#6988,#6966,#1460,.T.);
#9116=EDGE_CURVE('',#6964,#6996,#1461,.T.);
#9117=EDGE_CURVE('',#6962,#6995,#1462,.T.);
#9118=EDGE_CURVE('',#6992,#6959,#1463,.T.);
#9119=EDGE_CURVE('',#6994,#6960,#1464,.T.);
#9120=EDGE_CURVE('',#6958,#7002,#1465,.T.);
#9121=EDGE_CURVE('',#6956,#7001,#1466,.T.);
#9122=EDGE_CURVE('',#6998,#6953,#1467,.T.);
#9123=EDGE_CURVE('',#7000,#6954,#1468,.T.);
#9124=EDGE_CURVE('',#6952,#7008,#1469,.T.);
#9125=EDGE_CURVE('',#6950,#7007,#1470,.T.);
#9126=EDGE_CURVE('',#7004,#6947,#1471,.T.);
#9127=EDGE_CURVE('',#7006,#6948,#1472,.T.);
#9128=EDGE_CURVE('',#6946,#7014,#1473,.T.);
#9129=EDGE_CURVE('',#6944,#7013,#1474,.T.);
#9130=EDGE_CURVE('',#7010,#6941,#1475,.T.);
#9131=EDGE_CURVE('',#7012,#6942,#1476,.T.);
#9132=EDGE_CURVE('',#6940,#7020,#1477,.T.);
#9133=EDGE_CURVE('',#6938,#7019,#1478,.T.);
#9134=EDGE_CURVE('',#7064,#6935,#1479,.T.);
#9135=EDGE_CURVE('',#7066,#6936,#1480,.T.);
#9136=EDGE_CURVE('',#6934,#6978,#1481,.T.);
#9137=EDGE_CURVE('',#6932,#6977,#1482,.T.);
#9138=EDGE_CURVE('',#7022,#6929,#1483,.T.);
#9139=EDGE_CURVE('',#7024,#6930,#1484,.T.);
#9140=EDGE_CURVE('',#6928,#7032,#1485,.T.);
#9141=EDGE_CURVE('',#6926,#7031,#1486,.T.);
#9142=EDGE_CURVE('',#7028,#6923,#1487,.T.);
#9143=EDGE_CURVE('',#7030,#6924,#1488,.T.);
#9144=EDGE_CURVE('',#6922,#7038,#1489,.T.);
#9145=EDGE_CURVE('',#6920,#7037,#1490,.T.);
#9146=EDGE_CURVE('',#7034,#6917,#1491,.T.);
#9147=EDGE_CURVE('',#7036,#6918,#1492,.T.);
#9148=EDGE_CURVE('',#6916,#7044,#1493,.T.);
#9149=EDGE_CURVE('',#6914,#7043,#1494,.T.);
#9150=EDGE_CURVE('',#7040,#6911,#1495,.T.);
#9151=EDGE_CURVE('',#7042,#6912,#1496,.T.);
#9152=EDGE_CURVE('',#6910,#7050,#1497,.T.);
#9153=EDGE_CURVE('',#6908,#7049,#1498,.T.);
#9154=EDGE_CURVE('',#7046,#6905,#1499,.T.);
#9155=EDGE_CURVE('',#7048,#6906,#1500,.T.);
#9156=EDGE_CURVE('',#6904,#7056,#1501,.T.);
#9157=EDGE_CURVE('',#6902,#7055,#1502,.T.);
#9158=EDGE_CURVE('',#7052,#6899,#1503,.T.);
#9159=EDGE_CURVE('',#7054,#6900,#1504,.T.);
#9160=EDGE_CURVE('',#6898,#7062,#1505,.T.);
#9161=EDGE_CURVE('',#6896,#7061,#1506,.T.);
#9162=EDGE_CURVE('',#7058,#6893,#1507,.T.);
#9163=EDGE_CURVE('',#7060,#6894,#1508,.T.);
#9164=EDGE_CURVE('',#6892,#7068,#1509,.T.);
#9165=EDGE_CURVE('',#6890,#7067,#1510,.T.);
#9166=EDGE_CURVE('',#7023,#7069,#4515,.T.);
#9167=EDGE_CURVE('',#7069,#7069,#1511,.T.);
#9168=EDGE_CURVE('',#7070,#7070,#1512,.T.);
#9169=EDGE_CURVE('',#6887,#7070,#4516,.T.);
#9170=EDGE_CURVE('',#6824,#6885,#1513,.T.);
#9171=EDGE_CURVE('',#7071,#7071,#1514,.T.);
#9172=EDGE_CURVE('',#7071,#7021,#4517,.T.);
#9173=EDGE_CURVE('',#7072,#7073,#1515,.T.);
#9174=EDGE_CURVE('',#7074,#7074,#1516,.T.);
#9175=EDGE_CURVE('',#7074,#7075,#728,.T.);
#9176=EDGE_CURVE('',#7075,#7075,#1517,.T.);
#9177=EDGE_CURVE('',#7076,#7077,#4518,.T.);
#9178=EDGE_CURVE('',#7076,#7078,#729,.T.);
#9179=EDGE_CURVE('',#7078,#7079,#1518,.T.);
#9180=EDGE_CURVE('',#7079,#7077,#730,.T.);
#9181=EDGE_CURVE('',#7080,#7081,#4519,.T.);
#9182=EDGE_CURVE('',#7080,#7076,#731,.T.);
#9183=EDGE_CURVE('',#7077,#7081,#732,.T.);
#9184=EDGE_CURVE('',#7082,#7083,#4520,.T.);
#9185=EDGE_CURVE('',#7082,#7080,#733,.T.);
#9186=EDGE_CURVE('',#7081,#7083,#734,.T.);
#9187=EDGE_CURVE('',#7084,#7085,#4521,.T.);
#9188=EDGE_CURVE('',#7084,#7082,#735,.T.);
#9189=EDGE_CURVE('',#7083,#7085,#736,.T.);
#9190=EDGE_CURVE('',#7086,#7087,#4522,.T.);
#9191=EDGE_CURVE('',#7086,#7084,#737,.T.);
#9192=EDGE_CURVE('',#7085,#7087,#738,.T.);
#9193=EDGE_CURVE('',#7088,#7089,#4523,.T.);
#9194=EDGE_CURVE('',#7088,#7086,#739,.T.);
#9195=EDGE_CURVE('',#7087,#7089,#740,.T.);
#9196=EDGE_CURVE('',#7090,#7091,#4524,.T.);
#9197=EDGE_CURVE('',#7090,#7088,#741,.T.);
#9198=EDGE_CURVE('',#7089,#7091,#742,.T.);
#9199=EDGE_CURVE('',#7092,#7093,#4525,.T.);
#9200=EDGE_CURVE('',#7092,#7090,#743,.T.);
#9201=EDGE_CURVE('',#7091,#7093,#744,.T.);
#9202=EDGE_CURVE('',#7094,#7095,#4526,.T.);
#9203=EDGE_CURVE('',#7094,#7092,#745,.T.);
#9204=EDGE_CURVE('',#7093,#7095,#746,.T.);
#9205=EDGE_CURVE('',#7096,#7097,#4527,.T.);
#9206=EDGE_CURVE('',#7096,#7094,#747,.T.);
#9207=EDGE_CURVE('',#7095,#7097,#748,.T.);
#9208=EDGE_CURVE('',#7098,#7099,#4528,.T.);
#9209=EDGE_CURVE('',#7098,#7096,#749,.T.);
#9210=EDGE_CURVE('',#7097,#7099,#750,.T.);
#9211=EDGE_CURVE('',#7100,#7101,#4529,.T.);
#9212=EDGE_CURVE('',#7100,#7098,#751,.T.);
#9213=EDGE_CURVE('',#7099,#7101,#752,.T.);
#9214=EDGE_CURVE('',#7102,#7103,#4530,.T.);
#9215=EDGE_CURVE('',#7102,#7100,#753,.T.);
#9216=EDGE_CURVE('',#7101,#7103,#754,.T.);
#9217=EDGE_CURVE('',#7104,#7105,#4531,.T.);
#9218=EDGE_CURVE('',#7104,#7102,#755,.T.);
#9219=EDGE_CURVE('',#7103,#7105,#756,.T.);
#9220=EDGE_CURVE('',#7106,#7107,#4532,.T.);
#9221=EDGE_CURVE('',#7106,#7104,#757,.T.);
#9222=EDGE_CURVE('',#7105,#7107,#758,.T.);
#9223=EDGE_CURVE('',#7108,#7109,#4533,.T.);
#9224=EDGE_CURVE('',#7108,#7106,#759,.T.);
#9225=EDGE_CURVE('',#7107,#7109,#760,.T.);
#9226=EDGE_CURVE('',#7110,#7111,#4534,.T.);
#9227=EDGE_CURVE('',#7110,#7108,#761,.T.);
#9228=EDGE_CURVE('',#7109,#7111,#762,.T.);
#9229=EDGE_CURVE('',#7112,#7113,#4535,.T.);
#9230=EDGE_CURVE('',#7112,#7110,#763,.T.);
#9231=EDGE_CURVE('',#7111,#7113,#764,.T.);
#9232=EDGE_CURVE('',#7114,#7115,#4536,.T.);
#9233=EDGE_CURVE('',#7114,#7112,#765,.T.);
#9234=EDGE_CURVE('',#7113,#7115,#766,.T.);
#9235=EDGE_CURVE('',#7116,#7117,#4537,.T.);
#9236=EDGE_CURVE('',#7116,#7114,#767,.T.);
#9237=EDGE_CURVE('',#7115,#7117,#768,.T.);
#9238=EDGE_CURVE('',#7118,#7119,#4538,.T.);
#9239=EDGE_CURVE('',#7118,#7116,#769,.T.);
#9240=EDGE_CURVE('',#7117,#7119,#770,.T.);
#9241=EDGE_CURVE('',#7120,#7121,#4539,.T.);
#9242=EDGE_CURVE('',#7120,#7118,#771,.T.);
#9243=EDGE_CURVE('',#7119,#7121,#772,.T.);
#9244=EDGE_CURVE('',#7122,#7123,#4540,.T.);
#9245=EDGE_CURVE('',#7122,#7124,#773,.T.);
#9246=EDGE_CURVE('',#7125,#7124,#1519,.T.);
#9247=EDGE_CURVE('',#7123,#7125,#774,.T.);
#9248=EDGE_CURVE('',#7126,#7127,#4541,.T.);
#9249=EDGE_CURVE('',#7126,#7122,#775,.T.);
#9250=EDGE_CURVE('',#7127,#7123,#776,.T.);
#9251=EDGE_CURVE('',#7128,#7129,#4542,.T.);
#9252=EDGE_CURVE('',#7128,#7126,#777,.T.);
#9253=EDGE_CURVE('',#7129,#7127,#778,.T.);
#9254=EDGE_CURVE('',#7130,#7131,#4543,.T.);
#9255=EDGE_CURVE('',#7130,#7128,#779,.T.);
#9256=EDGE_CURVE('',#7131,#7129,#780,.T.);
#9257=EDGE_CURVE('',#7132,#7133,#4544,.T.);
#9258=EDGE_CURVE('',#7132,#7130,#781,.T.);
#9259=EDGE_CURVE('',#7133,#7131,#782,.T.);
#9260=EDGE_CURVE('',#7134,#7135,#4545,.T.);
#9261=EDGE_CURVE('',#7134,#7132,#783,.T.);
#9262=EDGE_CURVE('',#7135,#7133,#784,.T.);
#9263=EDGE_CURVE('',#7136,#7137,#4546,.T.);
#9264=EDGE_CURVE('',#7136,#7134,#785,.T.);
#9265=EDGE_CURVE('',#7137,#7135,#786,.T.);
#9266=EDGE_CURVE('',#7138,#7139,#4547,.T.);
#9267=EDGE_CURVE('',#7138,#7136,#787,.T.);
#9268=EDGE_CURVE('',#7139,#7137,#788,.T.);
#9269=EDGE_CURVE('',#7140,#7141,#4548,.T.);
#9270=EDGE_CURVE('',#7140,#7138,#789,.T.);
#9271=EDGE_CURVE('',#7141,#7139,#790,.T.);
#9272=EDGE_CURVE('',#7142,#7143,#4549,.T.);
#9273=EDGE_CURVE('',#7142,#7140,#791,.T.);
#9274=EDGE_CURVE('',#7143,#7141,#792,.T.);
#9275=EDGE_CURVE('',#7144,#7145,#4550,.T.);
#9276=EDGE_CURVE('',#7144,#7142,#793,.T.);
#9277=EDGE_CURVE('',#7145,#7143,#794,.T.);
#9278=EDGE_CURVE('',#7146,#7147,#4551,.T.);
#9279=EDGE_CURVE('',#7146,#7144,#795,.T.);
#9280=EDGE_CURVE('',#7147,#7145,#796,.T.);
#9281=EDGE_CURVE('',#7148,#7149,#4552,.T.);
#9282=EDGE_CURVE('',#7148,#7146,#797,.T.);
#9283=EDGE_CURVE('',#7149,#7147,#798,.T.);
#9284=EDGE_CURVE('',#7150,#7151,#4553,.T.);
#9285=EDGE_CURVE('',#7150,#7148,#799,.T.);
#9286=EDGE_CURVE('',#7151,#7149,#800,.T.);
#9287=EDGE_CURVE('',#7152,#7153,#4554,.T.);
#9288=EDGE_CURVE('',#7152,#7150,#801,.T.);
#9289=EDGE_CURVE('',#7153,#7151,#802,.T.);
#9290=EDGE_CURVE('',#7154,#7155,#4555,.T.);
#9291=EDGE_CURVE('',#7154,#7152,#803,.T.);
#9292=EDGE_CURVE('',#7155,#7153,#804,.T.);
#9293=EDGE_CURVE('',#7156,#7157,#4556,.T.);
#9294=EDGE_CURVE('',#7156,#7154,#805,.T.);
#9295=EDGE_CURVE('',#7157,#7155,#806,.T.);
#9296=EDGE_CURVE('',#7158,#7159,#4557,.T.);
#9297=EDGE_CURVE('',#7158,#7156,#807,.T.);
#9298=EDGE_CURVE('',#7159,#7157,#808,.T.);
#9299=EDGE_CURVE('',#7160,#7161,#4558,.T.);
#9300=EDGE_CURVE('',#7160,#7158,#809,.T.);
#9301=EDGE_CURVE('',#7161,#7159,#810,.T.);
#9302=EDGE_CURVE('',#7162,#7163,#4559,.T.);
#9303=EDGE_CURVE('',#7162,#7160,#811,.T.);
#9304=EDGE_CURVE('',#7163,#7161,#812,.T.);
#9305=EDGE_CURVE('',#7164,#7165,#4560,.T.);
#9306=EDGE_CURVE('',#7164,#7162,#813,.T.);
#9307=EDGE_CURVE('',#7165,#7163,#814,.T.);
#9308=EDGE_CURVE('',#7166,#7167,#4561,.T.);
#9309=EDGE_CURVE('',#7166,#7164,#815,.T.);
#9310=EDGE_CURVE('',#7167,#7165,#816,.T.);
#9311=EDGE_CURVE('',#7124,#7168,#817,.T.);
#9312=EDGE_CURVE('',#7169,#7168,#1520,.T.);
#9313=EDGE_CURVE('',#7170,#7169,#1521,.T.);
#9314=EDGE_CURVE('',#7170,#7125,#818,.T.);
#9315=EDGE_CURVE('',#7121,#7170,#819,.T.);
#9316=EDGE_CURVE('',#7171,#7079,#820,.T.);
#9317=EDGE_CURVE('',#7171,#7167,#821,.T.);
#9318=EDGE_CURVE('',#7079,#7172,#1522,.T.);
#9319=EDGE_CURVE('',#7172,#7078,#1523,.T.);
#9320=EDGE_CURVE('',#7078,#7173,#822,.T.);
#9321=EDGE_CURVE('',#7173,#7171,#1524,.T.);
#9322=EDGE_CURVE('',#7173,#7166,#823,.T.);
#9323=EDGE_CURVE('',#7168,#7120,#824,.T.);
#9324=EDGE_CURVE('',#7169,#7174,#1525,.T.);
#9325=EDGE_CURVE('',#7174,#7174,#1526,.T.);
#9326=EDGE_CURVE('',#7168,#7170,#1527,.T.);
#9327=EDGE_CURVE('',#7175,#7176,#4562,.T.);
#9328=EDGE_CURVE('',#7176,#7177,#4563,.T.);
#9329=EDGE_CURVE('',#7178,#7177,#1528,.T.);
#9330=EDGE_CURVE('',#7178,#7179,#4564,.T.);
#9331=EDGE_CURVE('',#7179,#7180,#4565,.T.);
#9332=EDGE_CURVE('',#7181,#7180,#1529,.T.);
#9333=EDGE_CURVE('',#7181,#7182,#4566,.T.);
#9334=EDGE_CURVE('',#7182,#7183,#4567,.T.);
#9335=EDGE_CURVE('',#7184,#7183,#1530,.T.);
#9336=EDGE_CURVE('',#7184,#7185,#4568,.T.);
#9337=EDGE_CURVE('',#7185,#7186,#4569,.T.);
#9338=EDGE_CURVE('',#7187,#7186,#1531,.T.);
#9339=EDGE_CURVE('',#7187,#7188,#4570,.T.);
#9340=EDGE_CURVE('',#7188,#7189,#4571,.T.);
#9341=EDGE_CURVE('',#7190,#7189,#1532,.T.);
#9342=EDGE_CURVE('',#7190,#7191,#4572,.T.);
#9343=EDGE_CURVE('',#7191,#7192,#4573,.T.);
#9344=EDGE_CURVE('',#7193,#7192,#1533,.T.);
#9345=EDGE_CURVE('',#7193,#7194,#4574,.T.);
#9346=EDGE_CURVE('',#7194,#7195,#4575,.T.);
#9347=EDGE_CURVE('',#7196,#7195,#1534,.T.);
#9348=EDGE_CURVE('',#7196,#7197,#4576,.T.);
#9349=EDGE_CURVE('',#7197,#7198,#4577,.T.);
#9350=EDGE_CURVE('',#7199,#7198,#1535,.T.);
#9351=EDGE_CURVE('',#7199,#7200,#4578,.T.);
#9352=EDGE_CURVE('',#7200,#7201,#4579,.T.);
#9353=EDGE_CURVE('',#7202,#7201,#1536,.T.);
#9354=EDGE_CURVE('',#7202,#7203,#4580,.T.);
#9355=EDGE_CURVE('',#7203,#7204,#4581,.T.);
#9356=EDGE_CURVE('',#7205,#7204,#1537,.T.);
#9357=EDGE_CURVE('',#7205,#7206,#4582,.T.);
#9358=EDGE_CURVE('',#7206,#7207,#4583,.T.);
#9359=EDGE_CURVE('',#7208,#7207,#1538,.T.);
#9360=EDGE_CURVE('',#7208,#7209,#4584,.T.);
#9361=EDGE_CURVE('',#7209,#7210,#4585,.T.);
#9362=EDGE_CURVE('',#7211,#7210,#1539,.T.);
#9363=EDGE_CURVE('',#7211,#7212,#4586,.T.);
#9364=EDGE_CURVE('',#7212,#7213,#4587,.T.);
#9365=EDGE_CURVE('',#7214,#7213,#1540,.T.);
#9366=EDGE_CURVE('',#7214,#7215,#4588,.T.);
#9367=EDGE_CURVE('',#7215,#7216,#4589,.T.);
#9368=EDGE_CURVE('',#7217,#7216,#1541,.T.);
#9369=EDGE_CURVE('',#7217,#7218,#4590,.T.);
#9370=EDGE_CURVE('',#7218,#7219,#4591,.T.);
#9371=EDGE_CURVE('',#7220,#7219,#1542,.T.);
#9372=EDGE_CURVE('',#7220,#7221,#4592,.T.);
#9373=EDGE_CURVE('',#7221,#7222,#4593,.T.);
#9374=EDGE_CURVE('',#7223,#7222,#1543,.T.);
#9375=EDGE_CURVE('',#7223,#7224,#4594,.T.);
#9376=EDGE_CURVE('',#7224,#7225,#4595,.T.);
#9377=EDGE_CURVE('',#7226,#7225,#1544,.T.);
#9378=EDGE_CURVE('',#7226,#7227,#4596,.T.);
#9379=EDGE_CURVE('',#7227,#7228,#4597,.T.);
#9380=EDGE_CURVE('',#7229,#7228,#1545,.T.);
#9381=EDGE_CURVE('',#7229,#7230,#4598,.T.);
#9382=EDGE_CURVE('',#7230,#7231,#4599,.T.);
#9383=EDGE_CURVE('',#7232,#7231,#1546,.T.);
#9384=EDGE_CURVE('',#7232,#7233,#4600,.T.);
#9385=EDGE_CURVE('',#7233,#7234,#4601,.T.);
#9386=EDGE_CURVE('',#7235,#7234,#1547,.T.);
#9387=EDGE_CURVE('',#7235,#7236,#4602,.T.);
#9388=EDGE_CURVE('',#7236,#7237,#4603,.T.);
#9389=EDGE_CURVE('',#7238,#7237,#1548,.T.);
#9390=EDGE_CURVE('',#7238,#7239,#4604,.T.);
#9391=EDGE_CURVE('',#7239,#7240,#4605,.T.);
#9392=EDGE_CURVE('',#7241,#7240,#1549,.T.);
#9393=EDGE_CURVE('',#7241,#7242,#4606,.T.);
#9394=EDGE_CURVE('',#7242,#7243,#4607,.T.);
#9395=EDGE_CURVE('',#7244,#7243,#1550,.T.);
#9396=EDGE_CURVE('',#7244,#7245,#4608,.T.);
#9397=EDGE_CURVE('',#7245,#7246,#4609,.T.);
#9398=EDGE_CURVE('',#7247,#7246,#1551,.T.);
#9399=EDGE_CURVE('',#7247,#7248,#4610,.T.);
#9400=EDGE_CURVE('',#7248,#7249,#4611,.T.);
#9401=EDGE_CURVE('',#7250,#7249,#1552,.T.);
#9402=EDGE_CURVE('',#7250,#7251,#4612,.T.);
#9403=EDGE_CURVE('',#7251,#7252,#4613,.T.);
#9404=EDGE_CURVE('',#7253,#7252,#1553,.T.);
#9405=EDGE_CURVE('',#7253,#7254,#4614,.T.);
#9406=EDGE_CURVE('',#7254,#7255,#4615,.T.);
#9407=EDGE_CURVE('',#7256,#7255,#1554,.T.);
#9408=EDGE_CURVE('',#7256,#7257,#4616,.T.);
#9409=EDGE_CURVE('',#7257,#7258,#4617,.T.);
#9410=EDGE_CURVE('',#7259,#7258,#1555,.T.);
#9411=EDGE_CURVE('',#7259,#7260,#4618,.T.);
#9412=EDGE_CURVE('',#7260,#7261,#4619,.T.);
#9413=EDGE_CURVE('',#7262,#7261,#1556,.T.);
#9414=EDGE_CURVE('',#7262,#7263,#4620,.T.);
#9415=EDGE_CURVE('',#7263,#7264,#4621,.T.);
#9416=EDGE_CURVE('',#7265,#7264,#1557,.T.);
#9417=EDGE_CURVE('',#7265,#7266,#4622,.T.);
#9418=EDGE_CURVE('',#7266,#7267,#4623,.T.);
#9419=EDGE_CURVE('',#7268,#7267,#1558,.T.);
#9420=EDGE_CURVE('',#7268,#7269,#4624,.T.);
#9421=EDGE_CURVE('',#7269,#7270,#4625,.T.);
#9422=EDGE_CURVE('',#7271,#7270,#1559,.T.);
#9423=EDGE_CURVE('',#7271,#7272,#4626,.T.);
#9424=EDGE_CURVE('',#7272,#7273,#4627,.T.);
#9425=EDGE_CURVE('',#7274,#7273,#1560,.T.);
#9426=EDGE_CURVE('',#7274,#7275,#4628,.T.);
#9427=EDGE_CURVE('',#7275,#7276,#4629,.T.);
#9428=EDGE_CURVE('',#7277,#7276,#1561,.T.);
#9429=EDGE_CURVE('',#7277,#7278,#4630,.T.);
#9430=EDGE_CURVE('',#7278,#7279,#4631,.T.);
#9431=EDGE_CURVE('',#7280,#7279,#1562,.T.);
#9432=EDGE_CURVE('',#7280,#7281,#4632,.T.);
#9433=EDGE_CURVE('',#7281,#7282,#4633,.T.);
#9434=EDGE_CURVE('',#7175,#7282,#1563,.T.);
#9435=EDGE_CURVE('',#7283,#7284,#4634,.T.);
#9436=EDGE_CURVE('',#7284,#7283,#1564,.T.);
#9437=EDGE_CURVE('',#7284,#7285,#4635,.T.);
#9438=EDGE_CURVE('',#7285,#7284,#1565,.T.);
#9439=EDGE_CURVE('',#7285,#7286,#4636,.T.);
#9440=EDGE_CURVE('',#7286,#7285,#1566,.T.);
#9441=EDGE_CURVE('',#7286,#7287,#4637,.T.);
#9442=EDGE_CURVE('',#7287,#7286,#1567,.T.);
#9443=EDGE_CURVE('',#7287,#7288,#4638,.T.);
#9444=EDGE_CURVE('',#7288,#7287,#1568,.T.);
#9445=EDGE_CURVE('',#7288,#7283,#4639,.T.);
#9446=EDGE_CURVE('',#7283,#7288,#1569,.T.);
#9447=EDGE_CURVE('',#7289,#7290,#4640,.T.);
#9448=EDGE_CURVE('',#7291,#7290,#1570,.T.);
#9449=EDGE_CURVE('',#7285,#7291,#252,.T.);
#9450=EDGE_CURVE('',#7292,#7284,#253,.T.);
#9451=EDGE_CURVE('',#7293,#7292,#1571,.T.);
#9452=EDGE_CURVE('',#7284,#7293,#254,.T.);
#9453=EDGE_CURVE('',#7294,#7283,#255,.T.);
#9454=EDGE_CURVE('',#7295,#7294,#1572,.T.);
#9455=EDGE_CURVE('',#7283,#7295,#256,.T.);
#9456=EDGE_CURVE('',#7296,#7288,#257,.T.);
#9457=EDGE_CURVE('',#7297,#7296,#1573,.T.);
#9458=EDGE_CURVE('',#7288,#7297,#258,.T.);
#9459=EDGE_CURVE('',#7298,#7287,#259,.T.);
#9460=EDGE_CURVE('',#7299,#7298,#1574,.T.);
#9461=EDGE_CURVE('',#7287,#7299,#260,.T.);
#9462=EDGE_CURVE('',#7300,#7286,#261,.T.);
#9463=EDGE_CURVE('',#7301,#7300,#1575,.T.);
#9464=EDGE_CURVE('',#7286,#7301,#262,.T.);
#9465=EDGE_CURVE('',#7302,#7285,#263,.T.);
#9466=EDGE_CURVE('',#7290,#7302,#1576,.T.);
#9467=EDGE_CURVE('',#7303,#7286,#4641,.T.);
#9468=EDGE_CURVE('',#7304,#7303,#4642,.T.);
#9469=EDGE_CURVE('',#7304,#7285,#4643,.T.);
#9470=EDGE_CURVE('',#7285,#7305,#4644,.T.);
#9471=EDGE_CURVE('',#7305,#7302,#4645,.T.);
#9472=EDGE_CURVE('',#7306,#7287,#4646,.T.);
#9473=EDGE_CURVE('',#7303,#7306,#4647,.T.);
#9474=EDGE_CURVE('',#7299,#7307,#4648,.T.);
#9475=EDGE_CURVE('',#7287,#7307,#4649,.T.);
#9476=EDGE_CURVE('',#7286,#7308,#4650,.T.);
#9477=EDGE_CURVE('',#7308,#7300,#4651,.T.);
#9478=EDGE_CURVE('',#7309,#7304,#4652,.T.);
#9479=EDGE_CURVE('',#7309,#7284,#4653,.T.);
#9480=EDGE_CURVE('',#7284,#7310,#4654,.T.);
#9481=EDGE_CURVE('',#7310,#7292,#4655,.T.);
#9482=EDGE_CURVE('',#7311,#7288,#4656,.T.);
#9483=EDGE_CURVE('',#7306,#7311,#4657,.T.);
#9484=EDGE_CURVE('',#7297,#7312,#4658,.T.);
#9485=EDGE_CURVE('',#7288,#7312,#4659,.T.);
#9486=EDGE_CURVE('',#7307,#7298,#4660,.T.);
#9487=EDGE_CURVE('',#7301,#7308,#4661,.T.);
#9488=EDGE_CURVE('',#7312,#7296,#4662,.T.);
#9489=EDGE_CURVE('',#7313,#7294,#4663,.T.);
#9490=EDGE_CURVE('',#7295,#7313,#4664,.T.);
#9491=EDGE_CURVE('',#7293,#7310,#4665,.T.);
#9492=EDGE_CURVE('',#7291,#7305,#4666,.T.);
#9493=EDGE_CURVE('',#7314,#7283,#4667,.T.);
#9494=EDGE_CURVE('',#7311,#7314,#4668,.T.);
#9495=EDGE_CURVE('',#7283,#7313,#4669,.T.);
#9496=EDGE_CURVE('',#7314,#7309,#4670,.T.);
#9497=EDGE_CURVE('',#7315,#7316,#264,.T.);
#9498=EDGE_CURVE('',#7315,#7176,#4671,.T.);
#9499=EDGE_CURVE('',#7316,#7175,#4672,.T.);
#9500=EDGE_CURVE('',#7317,#7315,#265,.T.);
#9501=EDGE_CURVE('',#7177,#7317,#4673,.T.);
#9502=EDGE_CURVE('',#7318,#7319,#266,.T.);
#9503=EDGE_CURVE('',#7318,#7182,#4674,.T.);
#9504=EDGE_CURVE('',#7319,#7181,#4675,.T.);
#9505=EDGE_CURVE('',#7320,#7318,#267,.T.);
#9506=EDGE_CURVE('',#7183,#7320,#4676,.T.);
#9507=EDGE_CURVE('',#7321,#7322,#268,.T.);
#9508=EDGE_CURVE('',#7321,#7188,#4677,.T.);
#9509=EDGE_CURVE('',#7322,#7187,#4678,.T.);
#9510=EDGE_CURVE('',#7323,#7321,#269,.T.);
#9511=EDGE_CURVE('',#7189,#7323,#4679,.T.);
#9512=EDGE_CURVE('',#7324,#7325,#270,.T.);
#9513=EDGE_CURVE('',#7324,#7194,#4680,.T.);
#9514=EDGE_CURVE('',#7325,#7193,#4681,.T.);
#9515=EDGE_CURVE('',#7326,#7324,#271,.T.);
#9516=EDGE_CURVE('',#7195,#7326,#4682,.T.);
#9517=EDGE_CURVE('',#7327,#7328,#272,.T.);
#9518=EDGE_CURVE('',#7327,#7200,#4683,.T.);
#9519=EDGE_CURVE('',#7328,#7199,#4684,.T.);
#9520=EDGE_CURVE('',#7329,#7327,#273,.T.);
#9521=EDGE_CURVE('',#7201,#7329,#4685,.T.);
#9522=EDGE_CURVE('',#7330,#7331,#274,.T.);
#9523=EDGE_CURVE('',#7330,#7206,#4686,.T.);
#9524=EDGE_CURVE('',#7331,#7205,#4687,.T.);
#9525=EDGE_CURVE('',#7332,#7330,#275,.T.);
#9526=EDGE_CURVE('',#7207,#7332,#4688,.T.);
#9527=EDGE_CURVE('',#7333,#7334,#276,.T.);
#9528=EDGE_CURVE('',#7333,#7212,#4689,.T.);
#9529=EDGE_CURVE('',#7334,#7211,#4690,.T.);
#9530=EDGE_CURVE('',#7335,#7333,#277,.T.);
#9531=EDGE_CURVE('',#7213,#7335,#4691,.T.);
#9532=EDGE_CURVE('',#7336,#7337,#278,.T.);
#9533=EDGE_CURVE('',#7336,#7218,#4692,.T.);
#9534=EDGE_CURVE('',#7337,#7217,#4693,.T.);
#9535=EDGE_CURVE('',#7338,#7336,#279,.T.);
#9536=EDGE_CURVE('',#7219,#7338,#4694,.T.);
#9537=EDGE_CURVE('',#7339,#7340,#280,.T.);
#9538=EDGE_CURVE('',#7339,#7224,#4695,.T.);
#9539=EDGE_CURVE('',#7340,#7223,#4696,.T.);
#9540=EDGE_CURVE('',#7341,#7339,#281,.T.);
#9541=EDGE_CURVE('',#7225,#7341,#4697,.T.);
#9542=EDGE_CURVE('',#7342,#7343,#282,.T.);
#9543=EDGE_CURVE('',#7342,#7227,#4698,.T.);
#9544=EDGE_CURVE('',#7343,#7226,#4699,.T.);
#9545=EDGE_CURVE('',#7344,#7342,#283,.T.);
#9546=EDGE_CURVE('',#7228,#7344,#4700,.T.);
#9547=EDGE_CURVE('',#7345,#7346,#284,.T.);
#9548=EDGE_CURVE('',#7345,#7233,#4701,.T.);
#9549=EDGE_CURVE('',#7346,#7232,#4702,.T.);
#9550=EDGE_CURVE('',#7347,#7345,#285,.T.);
#9551=EDGE_CURVE('',#7234,#7347,#4703,.T.);
#9552=EDGE_CURVE('',#7348,#7349,#286,.T.);
#9553=EDGE_CURVE('',#7348,#7239,#4704,.T.);
#9554=EDGE_CURVE('',#7349,#7238,#4705,.T.);
#9555=EDGE_CURVE('',#7350,#7348,#287,.T.);
#9556=EDGE_CURVE('',#7240,#7350,#4706,.T.);
#9557=EDGE_CURVE('',#7351,#7352,#288,.T.);
#9558=EDGE_CURVE('',#7351,#7245,#4707,.T.);
#9559=EDGE_CURVE('',#7352,#7244,#4708,.T.);
#9560=EDGE_CURVE('',#7353,#7351,#289,.T.);
#9561=EDGE_CURVE('',#7246,#7353,#4709,.T.);
#9562=EDGE_CURVE('',#7354,#7355,#290,.T.);
#9563=EDGE_CURVE('',#7354,#7251,#4710,.T.);
#9564=EDGE_CURVE('',#7355,#7250,#4711,.T.);
#9565=EDGE_CURVE('',#7356,#7354,#291,.T.);
#9566=EDGE_CURVE('',#7252,#7356,#4712,.T.);
#9567=EDGE_CURVE('',#7357,#7358,#292,.T.);
#9568=EDGE_CURVE('',#7357,#7257,#4713,.T.);
#9569=EDGE_CURVE('',#7358,#7256,#4714,.T.);
#9570=EDGE_CURVE('',#7359,#7357,#293,.T.);
#9571=EDGE_CURVE('',#7258,#7359,#4715,.T.);
#9572=EDGE_CURVE('',#7360,#7361,#294,.T.);
#9573=EDGE_CURVE('',#7360,#7263,#4716,.T.);
#9574=EDGE_CURVE('',#7361,#7262,#4717,.T.);
#9575=EDGE_CURVE('',#7362,#7360,#295,.T.);
#9576=EDGE_CURVE('',#7264,#7362,#4718,.T.);
#9577=EDGE_CURVE('',#7363,#7364,#296,.T.);
#9578=EDGE_CURVE('',#7363,#7269,#4719,.T.);
#9579=EDGE_CURVE('',#7364,#7268,#4720,.T.);
#9580=EDGE_CURVE('',#7365,#7363,#297,.T.);
#9581=EDGE_CURVE('',#7270,#7365,#4721,.T.);
#9582=EDGE_CURVE('',#7366,#7367,#298,.T.);
#9583=EDGE_CURVE('',#7366,#7275,#4722,.T.);
#9584=EDGE_CURVE('',#7367,#7274,#4723,.T.);
#9585=EDGE_CURVE('',#7368,#7366,#299,.T.);
#9586=EDGE_CURVE('',#7276,#7368,#4724,.T.);
#9587=EDGE_CURVE('',#7369,#7370,#300,.T.);
#9588=EDGE_CURVE('',#7369,#7272,#4725,.T.);
#9589=EDGE_CURVE('',#7370,#7271,#4726,.T.);
#9590=EDGE_CURVE('',#7371,#7369,#301,.T.);
#9591=EDGE_CURVE('',#7273,#7371,#4727,.T.);
#9592=EDGE_CURVE('',#7372,#7373,#302,.T.);
#9593=EDGE_CURVE('',#7372,#7266,#4728,.T.);
#9594=EDGE_CURVE('',#7373,#7265,#4729,.T.);
#9595=EDGE_CURVE('',#7374,#7372,#303,.T.);
#9596=EDGE_CURVE('',#7267,#7374,#4730,.T.);
#9597=EDGE_CURVE('',#7375,#7376,#304,.T.);
#9598=EDGE_CURVE('',#7375,#7260,#4731,.T.);
#9599=EDGE_CURVE('',#7376,#7259,#4732,.T.);
#9600=EDGE_CURVE('',#7377,#7375,#305,.T.);
#9601=EDGE_CURVE('',#7261,#7377,#4733,.T.);
#9602=EDGE_CURVE('',#7378,#7379,#306,.T.);
#9603=EDGE_CURVE('',#7378,#7254,#4734,.T.);
#9604=EDGE_CURVE('',#7379,#7253,#4735,.T.);
#9605=EDGE_CURVE('',#7380,#7378,#307,.T.);
#9606=EDGE_CURVE('',#7255,#7380,#4736,.T.);
#9607=EDGE_CURVE('',#7381,#7382,#308,.T.);
#9608=EDGE_CURVE('',#7381,#7248,#4737,.T.);
#9609=EDGE_CURVE('',#7382,#7247,#4738,.T.);
#9610=EDGE_CURVE('',#7383,#7381,#309,.T.);
#9611=EDGE_CURVE('',#7249,#7383,#4739,.T.);
#9612=EDGE_CURVE('',#7384,#7385,#310,.T.);
#9613=EDGE_CURVE('',#7384,#7242,#4740,.T.);
#9614=EDGE_CURVE('',#7385,#7241,#4741,.T.);
#9615=EDGE_CURVE('',#7386,#7384,#311,.T.);
#9616=EDGE_CURVE('',#7243,#7386,#4742,.T.);
#9617=EDGE_CURVE('',#7387,#7388,#312,.T.);
#9618=EDGE_CURVE('',#7387,#7236,#4743,.T.);
#9619=EDGE_CURVE('',#7388,#7235,#4744,.T.);
#9620=EDGE_CURVE('',#7389,#7387,#313,.T.);
#9621=EDGE_CURVE('',#7237,#7389,#4745,.T.);
#9622=EDGE_CURVE('',#7390,#7391,#314,.T.);
#9623=EDGE_CURVE('',#7390,#7230,#4746,.T.);
#9624=EDGE_CURVE('',#7391,#7229,#4747,.T.);
#9625=EDGE_CURVE('',#7392,#7390,#315,.T.);
#9626=EDGE_CURVE('',#7231,#7392,#4748,.T.);
#9627=EDGE_CURVE('',#7393,#7394,#316,.T.);
#9628=EDGE_CURVE('',#7393,#7278,#4749,.T.);
#9629=EDGE_CURVE('',#7394,#7277,#4750,.T.);
#9630=EDGE_CURVE('',#7395,#7393,#317,.T.);
#9631=EDGE_CURVE('',#7279,#7395,#4751,.T.);
#9632=EDGE_CURVE('',#7396,#7397,#318,.T.);
#9633=EDGE_CURVE('',#7396,#7221,#4752,.T.);
#9634=EDGE_CURVE('',#7397,#7220,#4753,.T.);
#9635=EDGE_CURVE('',#7398,#7396,#319,.T.);
#9636=EDGE_CURVE('',#7222,#7398,#4754,.T.);
#9637=EDGE_CURVE('',#7399,#7400,#320,.T.);
#9638=EDGE_CURVE('',#7399,#7215,#4755,.T.);
#9639=EDGE_CURVE('',#7400,#7214,#4756,.T.);
#9640=EDGE_CURVE('',#7401,#7399,#321,.T.);
#9641=EDGE_CURVE('',#7216,#7401,#4757,.T.);
#9642=EDGE_CURVE('',#7402,#7403,#322,.T.);
#9643=EDGE_CURVE('',#7402,#7209,#4758,.T.);
#9644=EDGE_CURVE('',#7403,#7208,#4759,.T.);
#9645=EDGE_CURVE('',#7404,#7402,#323,.T.);
#9646=EDGE_CURVE('',#7210,#7404,#4760,.T.);
#9647=EDGE_CURVE('',#7405,#7406,#324,.T.);
#9648=EDGE_CURVE('',#7405,#7203,#4761,.T.);
#9649=EDGE_CURVE('',#7406,#7202,#4762,.T.);
#9650=EDGE_CURVE('',#7407,#7405,#325,.T.);
#9651=EDGE_CURVE('',#7204,#7407,#4763,.T.);
#9652=EDGE_CURVE('',#7408,#7409,#326,.T.);
#9653=EDGE_CURVE('',#7408,#7197,#4764,.T.);
#9654=EDGE_CURVE('',#7409,#7196,#4765,.T.);
#9655=EDGE_CURVE('',#7410,#7408,#327,.T.);
#9656=EDGE_CURVE('',#7198,#7410,#4766,.T.);
#9657=EDGE_CURVE('',#7411,#7412,#328,.T.);
#9658=EDGE_CURVE('',#7411,#7191,#4767,.T.);
#9659=EDGE_CURVE('',#7412,#7190,#4768,.T.);
#9660=EDGE_CURVE('',#7413,#7411,#329,.T.);
#9661=EDGE_CURVE('',#7192,#7413,#4769,.T.);
#9662=EDGE_CURVE('',#7414,#7415,#330,.T.);
#9663=EDGE_CURVE('',#7414,#7185,#4770,.T.);
#9664=EDGE_CURVE('',#7415,#7184,#4771,.T.);
#9665=EDGE_CURVE('',#7416,#7414,#331,.T.);
#9666=EDGE_CURVE('',#7186,#7416,#4772,.T.);
#9667=EDGE_CURVE('',#7417,#7418,#332,.T.);
#9668=EDGE_CURVE('',#7417,#7179,#4773,.T.);
#9669=EDGE_CURVE('',#7418,#7178,#4774,.T.);
#9670=EDGE_CURVE('',#7419,#7417,#333,.T.);
#9671=EDGE_CURVE('',#7180,#7419,#4775,.T.);
#9672=EDGE_CURVE('',#7420,#7421,#334,.T.);
#9673=EDGE_CURVE('',#7420,#7281,#4776,.T.);
#9674=EDGE_CURVE('',#7421,#7280,#4777,.T.);
#9675=EDGE_CURVE('',#7422,#7420,#335,.T.);
#9676=EDGE_CURVE('',#7282,#7422,#4778,.T.);
#9677=EDGE_CURVE('',#7421,#7395,#1577,.T.);
#9678=EDGE_CURVE('',#7394,#7368,#1578,.T.);
#9679=EDGE_CURVE('',#7367,#7371,#1579,.T.);
#9680=EDGE_CURVE('',#7370,#7365,#1580,.T.);
#9681=EDGE_CURVE('',#7364,#7374,#1581,.T.);
#9682=EDGE_CURVE('',#7373,#7362,#1582,.T.);
#9683=EDGE_CURVE('',#7361,#7377,#1583,.T.);
#9684=EDGE_CURVE('',#7376,#7359,#1584,.T.);
#9685=EDGE_CURVE('',#7358,#7380,#1585,.T.);
#9686=EDGE_CURVE('',#7379,#7356,#1586,.T.);
#9687=EDGE_CURVE('',#7355,#7383,#1587,.T.);
#9688=EDGE_CURVE('',#7382,#7353,#1588,.T.);
#9689=EDGE_CURVE('',#7352,#7386,#1589,.T.);
#9690=EDGE_CURVE('',#7385,#7350,#1590,.T.);
#9691=EDGE_CURVE('',#7349,#7389,#1591,.T.);
#9692=EDGE_CURVE('',#7388,#7347,#1592,.T.);
#9693=EDGE_CURVE('',#7346,#7392,#1593,.T.);
#9694=EDGE_CURVE('',#7391,#7344,#1594,.T.);
#9695=EDGE_CURVE('',#7343,#7341,#1595,.T.);
#9696=EDGE_CURVE('',#7340,#7398,#1596,.T.);
#9697=EDGE_CURVE('',#7397,#7338,#1597,.T.);
#9698=EDGE_CURVE('',#7337,#7401,#1598,.T.);
#9699=EDGE_CURVE('',#7400,#7335,#1599,.T.);
#9700=EDGE_CURVE('',#7334,#7404,#1600,.T.);
#9701=EDGE_CURVE('',#7403,#7332,#1601,.T.);
#9702=EDGE_CURVE('',#7331,#7407,#1602,.T.);
#9703=EDGE_CURVE('',#7406,#7329,#1603,.T.);
#9704=EDGE_CURVE('',#7328,#7410,#1604,.T.);
#9705=EDGE_CURVE('',#7409,#7326,#1605,.T.);
#9706=EDGE_CURVE('',#7325,#7413,#1606,.T.);
#9707=EDGE_CURVE('',#7412,#7323,#1607,.T.);
#9708=EDGE_CURVE('',#7322,#7416,#1608,.T.);
#9709=EDGE_CURVE('',#7415,#7320,#1609,.T.);
#9710=EDGE_CURVE('',#7319,#7419,#1610,.T.);
#9711=EDGE_CURVE('',#7418,#7317,#1611,.T.);
#9712=EDGE_CURVE('',#7316,#7422,#1612,.T.);
#9713=EDGE_CURVE('',#7423,#7423,#1613,.T.);
#9714=EDGE_CURVE('',#7172,#7423,#4779,.T.);
#9715=EDGE_CURVE('',#7424,#7424,#1614,.T.);
#9716=EDGE_CURVE('',#7424,#7339,#4780,.T.);
#9717=EDGE_CURVE('',#7425,#7426,#4781,.T.);
#9718=EDGE_CURVE('',#7425,#7427,#825,.T.);
#9719=EDGE_CURVE('',#7427,#7428,#1615,.T.);
#9720=EDGE_CURVE('',#7428,#7426,#826,.T.);
#9721=EDGE_CURVE('',#7429,#7430,#4782,.T.);
#9722=EDGE_CURVE('',#7429,#7425,#827,.T.);
#9723=EDGE_CURVE('',#7426,#7430,#828,.T.);
#9724=EDGE_CURVE('',#7431,#7432,#4783,.T.);
#9725=EDGE_CURVE('',#7431,#7429,#829,.T.);
#9726=EDGE_CURVE('',#7430,#7432,#830,.T.);
#9727=EDGE_CURVE('',#7433,#7434,#4784,.T.);
#9728=EDGE_CURVE('',#7433,#7431,#831,.T.);
#9729=EDGE_CURVE('',#7432,#7434,#832,.T.);
#9730=EDGE_CURVE('',#7435,#7436,#4785,.T.);
#9731=EDGE_CURVE('',#7435,#7433,#833,.T.);
#9732=EDGE_CURVE('',#7434,#7436,#834,.T.);
#9733=EDGE_CURVE('',#7437,#7438,#4786,.T.);
#9734=EDGE_CURVE('',#7437,#7435,#835,.T.);
#9735=EDGE_CURVE('',#7436,#7438,#836,.T.);
#9736=EDGE_CURVE('',#7439,#7440,#4787,.T.);
#9737=EDGE_CURVE('',#7439,#7437,#837,.T.);
#9738=EDGE_CURVE('',#7438,#7440,#838,.T.);
#9739=EDGE_CURVE('',#7441,#7442,#4788,.T.);
#9740=EDGE_CURVE('',#7441,#7439,#839,.T.);
#9741=EDGE_CURVE('',#7440,#7442,#840,.T.);
#9742=EDGE_CURVE('',#7443,#7444,#4789,.T.);
#9743=EDGE_CURVE('',#7443,#7441,#841,.T.);
#9744=EDGE_CURVE('',#7442,#7444,#842,.T.);
#9745=EDGE_CURVE('',#7445,#7446,#4790,.T.);
#9746=EDGE_CURVE('',#7445,#7443,#843,.T.);
#9747=EDGE_CURVE('',#7444,#7446,#844,.T.);
#9748=EDGE_CURVE('',#7447,#7448,#4791,.T.);
#9749=EDGE_CURVE('',#7447,#7445,#845,.T.);
#9750=EDGE_CURVE('',#7446,#7448,#846,.T.);
#9751=EDGE_CURVE('',#7449,#7450,#4792,.T.);
#9752=EDGE_CURVE('',#7449,#7451,#847,.T.);
#9753=EDGE_CURVE('',#7452,#7451,#1616,.T.);
#9754=EDGE_CURVE('',#7450,#7452,#848,.T.);
#9755=EDGE_CURVE('',#7453,#7454,#4793,.T.);
#9756=EDGE_CURVE('',#7453,#7449,#849,.T.);
#9757=EDGE_CURVE('',#7454,#7450,#850,.T.);
#9758=EDGE_CURVE('',#7455,#7456,#4794,.T.);
#9759=EDGE_CURVE('',#7455,#7453,#851,.T.);
#9760=EDGE_CURVE('',#7456,#7454,#852,.T.);
#9761=EDGE_CURVE('',#7457,#7458,#4795,.T.);
#9762=EDGE_CURVE('',#7457,#7455,#853,.T.);
#9763=EDGE_CURVE('',#7458,#7456,#854,.T.);
#9764=EDGE_CURVE('',#7459,#7460,#4796,.T.);
#9765=EDGE_CURVE('',#7459,#7457,#855,.T.);
#9766=EDGE_CURVE('',#7460,#7458,#856,.T.);
#9767=EDGE_CURVE('',#7461,#7462,#4797,.T.);
#9768=EDGE_CURVE('',#7461,#7459,#857,.T.);
#9769=EDGE_CURVE('',#7462,#7460,#858,.T.);
#9770=EDGE_CURVE('',#7463,#7464,#4798,.T.);
#9771=EDGE_CURVE('',#7463,#7461,#859,.T.);
#9772=EDGE_CURVE('',#7464,#7462,#860,.T.);
#9773=EDGE_CURVE('',#7465,#7466,#4799,.T.);
#9774=EDGE_CURVE('',#7465,#7463,#861,.T.);
#9775=EDGE_CURVE('',#7466,#7464,#862,.T.);
#9776=EDGE_CURVE('',#7467,#7468,#4800,.T.);
#9777=EDGE_CURVE('',#7467,#7465,#863,.T.);
#9778=EDGE_CURVE('',#7468,#7466,#864,.T.);
#9779=EDGE_CURVE('',#7469,#7470,#4801,.T.);
#9780=EDGE_CURVE('',#7469,#7467,#865,.T.);
#9781=EDGE_CURVE('',#7470,#7468,#866,.T.);
#9782=EDGE_CURVE('',#7471,#7472,#4802,.T.);
#9783=EDGE_CURVE('',#7471,#7469,#867,.T.);
#9784=EDGE_CURVE('',#7472,#7470,#868,.T.);
#9785=EDGE_CURVE('',#7473,#7452,#869,.T.);
#9786=EDGE_CURVE('',#7448,#7473,#870,.T.);
#9787=EDGE_CURVE('',#7474,#7428,#871,.T.);
#9788=EDGE_CURVE('',#7474,#7472,#872,.T.);
#9789=EDGE_CURVE('',#7428,#7475,#1617,.T.);
#9790=EDGE_CURVE('',#7475,#7427,#1618,.T.);
#9791=EDGE_CURVE('',#7427,#7476,#873,.T.);
#9792=EDGE_CURVE('',#7476,#7474,#1619,.T.);
#9793=EDGE_CURVE('',#7476,#7471,#874,.T.);
#9794=EDGE_CURVE('',#7451,#7477,#875,.T.);
#9795=EDGE_CURVE('',#7477,#7447,#876,.T.);
#9796=EDGE_CURVE('',#7478,#7479,#336,.T.);
#9797=EDGE_CURVE('',#7478,#7480,#4803,.T.);
#9798=EDGE_CURVE('',#7481,#7480,#337,.T.);
#9799=EDGE_CURVE('',#7479,#7481,#4804,.T.);
#9800=EDGE_CURVE('',#7482,#7478,#338,.T.);
#9801=EDGE_CURVE('',#7483,#7482,#4805,.T.);
#9802=EDGE_CURVE('',#7480,#7483,#339,.T.);
#9803=EDGE_CURVE('',#7484,#7485,#340,.T.);
#9804=EDGE_CURVE('',#7484,#7486,#4806,.T.);
#9805=EDGE_CURVE('',#7487,#7486,#341,.T.);
#9806=EDGE_CURVE('',#7485,#7487,#4807,.T.);
#9807=EDGE_CURVE('',#7488,#7484,#342,.T.);
#9808=EDGE_CURVE('',#7489,#7488,#4808,.T.);
#9809=EDGE_CURVE('',#7486,#7489,#343,.T.);
#9810=EDGE_CURVE('',#7490,#7491,#344,.T.);
#9811=EDGE_CURVE('',#7490,#7492,#4809,.T.);
#9812=EDGE_CURVE('',#7493,#7492,#345,.T.);
#9813=EDGE_CURVE('',#7491,#7493,#4810,.T.);
#9814=EDGE_CURVE('',#7494,#7490,#346,.T.);
#9815=EDGE_CURVE('',#7495,#7494,#4811,.T.);
#9816=EDGE_CURVE('',#7492,#7495,#347,.T.);
#9817=EDGE_CURVE('',#7496,#7497,#348,.T.);
#9818=EDGE_CURVE('',#7496,#7498,#4812,.T.);
#9819=EDGE_CURVE('',#7499,#7498,#349,.T.);
#9820=EDGE_CURVE('',#7497,#7499,#4813,.T.);
#9821=EDGE_CURVE('',#7500,#7496,#350,.T.);
#9822=EDGE_CURVE('',#7501,#7500,#4814,.T.);
#9823=EDGE_CURVE('',#7498,#7501,#351,.T.);
#9824=EDGE_CURVE('',#7502,#7503,#352,.T.);
#9825=EDGE_CURVE('',#7502,#7504,#4815,.T.);
#9826=EDGE_CURVE('',#7505,#7504,#353,.T.);
#9827=EDGE_CURVE('',#7503,#7505,#4816,.T.);
#9828=EDGE_CURVE('',#7506,#7502,#354,.T.);
#9829=EDGE_CURVE('',#7507,#7506,#4817,.T.);
#9830=EDGE_CURVE('',#7504,#7507,#355,.T.);
#9831=EDGE_CURVE('',#7508,#7509,#356,.T.);
#9832=EDGE_CURVE('',#7508,#7510,#4818,.T.);
#9833=EDGE_CURVE('',#7511,#7510,#357,.T.);
#9834=EDGE_CURVE('',#7509,#7511,#4819,.T.);
#9835=EDGE_CURVE('',#7512,#7508,#358,.T.);
#9836=EDGE_CURVE('',#7513,#7512,#4820,.T.);
#9837=EDGE_CURVE('',#7510,#7513,#359,.T.);
#9838=EDGE_CURVE('',#7514,#7515,#360,.T.);
#9839=EDGE_CURVE('',#7514,#7516,#4821,.T.);
#9840=EDGE_CURVE('',#7517,#7516,#361,.T.);
#9841=EDGE_CURVE('',#7515,#7517,#4822,.T.);
#9842=EDGE_CURVE('',#7518,#7514,#362,.T.);
#9843=EDGE_CURVE('',#7519,#7518,#4823,.T.);
#9844=EDGE_CURVE('',#7516,#7519,#363,.T.);
#9845=EDGE_CURVE('',#7520,#7521,#364,.T.);
#9846=EDGE_CURVE('',#7520,#7522,#4824,.T.);
#9847=EDGE_CURVE('',#7523,#7522,#365,.T.);
#9848=EDGE_CURVE('',#7521,#7523,#4825,.T.);
#9849=EDGE_CURVE('',#7524,#7520,#366,.T.);
#9850=EDGE_CURVE('',#7525,#7524,#4826,.T.);
#9851=EDGE_CURVE('',#7522,#7525,#367,.T.);
#9852=EDGE_CURVE('',#7526,#7527,#368,.T.);
#9853=EDGE_CURVE('',#7526,#7528,#4827,.T.);
#9854=EDGE_CURVE('',#7529,#7528,#369,.T.);
#9855=EDGE_CURVE('',#7527,#7529,#4828,.T.);
#9856=EDGE_CURVE('',#7530,#7526,#370,.T.);
#9857=EDGE_CURVE('',#7531,#7530,#4829,.T.);
#9858=EDGE_CURVE('',#7528,#7531,#371,.T.);
#9859=EDGE_CURVE('',#7532,#7533,#372,.T.);
#9860=EDGE_CURVE('',#7532,#7534,#4830,.T.);
#9861=EDGE_CURVE('',#7535,#7534,#373,.T.);
#9862=EDGE_CURVE('',#7533,#7535,#4831,.T.);
#9863=EDGE_CURVE('',#7536,#7532,#374,.T.);
#9864=EDGE_CURVE('',#7537,#7536,#4832,.T.);
#9865=EDGE_CURVE('',#7534,#7537,#375,.T.);
#9866=EDGE_CURVE('',#7538,#7539,#376,.T.);
#9867=EDGE_CURVE('',#7538,#7540,#4833,.T.);
#9868=EDGE_CURVE('',#7541,#7540,#377,.T.);
#9869=EDGE_CURVE('',#7539,#7541,#4834,.T.);
#9870=EDGE_CURVE('',#7542,#7538,#378,.T.);
#9871=EDGE_CURVE('',#7543,#7542,#4835,.T.);
#9872=EDGE_CURVE('',#7540,#7543,#379,.T.);
#9873=EDGE_CURVE('',#7544,#7545,#380,.T.);
#9874=EDGE_CURVE('',#7544,#7546,#4836,.T.);
#9875=EDGE_CURVE('',#7547,#7546,#381,.T.);
#9876=EDGE_CURVE('',#7545,#7547,#4837,.T.);
#9877=EDGE_CURVE('',#7548,#7544,#382,.T.);
#9878=EDGE_CURVE('',#7549,#7548,#4838,.T.);
#9879=EDGE_CURVE('',#7546,#7549,#383,.T.);
#9880=EDGE_CURVE('',#7550,#7551,#384,.T.);
#9881=EDGE_CURVE('',#7550,#7552,#4839,.T.);
#9882=EDGE_CURVE('',#7553,#7552,#385,.T.);
#9883=EDGE_CURVE('',#7551,#7553,#4840,.T.);
#9884=EDGE_CURVE('',#7554,#7550,#386,.T.);
#9885=EDGE_CURVE('',#7555,#7554,#4841,.T.);
#9886=EDGE_CURVE('',#7552,#7555,#387,.T.);
#9887=EDGE_CURVE('',#7556,#7557,#388,.T.);
#9888=EDGE_CURVE('',#7556,#7558,#4842,.T.);
#9889=EDGE_CURVE('',#7559,#7558,#389,.T.);
#9890=EDGE_CURVE('',#7557,#7559,#4843,.T.);
#9891=EDGE_CURVE('',#7560,#7556,#390,.T.);
#9892=EDGE_CURVE('',#7561,#7560,#4844,.T.);
#9893=EDGE_CURVE('',#7558,#7561,#391,.T.);
#9894=EDGE_CURVE('',#7562,#7563,#392,.T.);
#9895=EDGE_CURVE('',#7562,#7564,#4845,.T.);
#9896=EDGE_CURVE('',#7565,#7564,#393,.T.);
#9897=EDGE_CURVE('',#7563,#7565,#4846,.T.);
#9898=EDGE_CURVE('',#7566,#7562,#394,.T.);
#9899=EDGE_CURVE('',#7567,#7566,#4847,.T.);
#9900=EDGE_CURVE('',#7564,#7567,#395,.T.);
#9901=EDGE_CURVE('',#7568,#7569,#396,.T.);
#9902=EDGE_CURVE('',#7568,#7570,#4848,.T.);
#9903=EDGE_CURVE('',#7571,#7570,#397,.T.);
#9904=EDGE_CURVE('',#7569,#7571,#4849,.T.);
#9905=EDGE_CURVE('',#7572,#7568,#398,.T.);
#9906=EDGE_CURVE('',#7573,#7572,#4850,.T.);
#9907=EDGE_CURVE('',#7570,#7573,#399,.T.);
#9908=EDGE_CURVE('',#7574,#7575,#400,.T.);
#9909=EDGE_CURVE('',#7574,#7576,#4851,.T.);
#9910=EDGE_CURVE('',#7577,#7576,#401,.T.);
#9911=EDGE_CURVE('',#7575,#7577,#4852,.T.);
#9912=EDGE_CURVE('',#7578,#7574,#402,.T.);
#9913=EDGE_CURVE('',#7579,#7578,#4853,.T.);
#9914=EDGE_CURVE('',#7576,#7579,#403,.T.);
#9915=EDGE_CURVE('',#7580,#7581,#404,.T.);
#9916=EDGE_CURVE('',#7580,#7582,#4854,.T.);
#9917=EDGE_CURVE('',#7583,#7582,#405,.T.);
#9918=EDGE_CURVE('',#7581,#7583,#4855,.T.);
#9919=EDGE_CURVE('',#7584,#7580,#406,.T.);
#9920=EDGE_CURVE('',#7585,#7584,#4856,.T.);
#9921=EDGE_CURVE('',#7582,#7585,#407,.T.);
#9922=EDGE_CURVE('',#7586,#7587,#408,.T.);
#9923=EDGE_CURVE('',#7586,#7588,#4857,.T.);
#9924=EDGE_CURVE('',#7589,#7588,#409,.T.);
#9925=EDGE_CURVE('',#7587,#7589,#4858,.T.);
#9926=EDGE_CURVE('',#7590,#7586,#410,.T.);
#9927=EDGE_CURVE('',#7591,#7590,#4859,.T.);
#9928=EDGE_CURVE('',#7588,#7591,#411,.T.);
#9929=EDGE_CURVE('',#7592,#7593,#412,.T.);
#9930=EDGE_CURVE('',#7592,#7594,#4860,.T.);
#9931=EDGE_CURVE('',#7595,#7594,#413,.T.);
#9932=EDGE_CURVE('',#7593,#7595,#4861,.T.);
#9933=EDGE_CURVE('',#7596,#7592,#414,.T.);
#9934=EDGE_CURVE('',#7597,#7596,#4862,.T.);
#9935=EDGE_CURVE('',#7594,#7597,#415,.T.);
#9936=EDGE_CURVE('',#7598,#7599,#416,.T.);
#9937=EDGE_CURVE('',#7598,#7600,#4863,.T.);
#9938=EDGE_CURVE('',#7601,#7600,#417,.T.);
#9939=EDGE_CURVE('',#7599,#7601,#4864,.T.);
#9940=EDGE_CURVE('',#7602,#7598,#418,.T.);
#9941=EDGE_CURVE('',#7603,#7602,#4865,.T.);
#9942=EDGE_CURVE('',#7600,#7603,#419,.T.);
#9943=EDGE_CURVE('',#7604,#7605,#420,.T.);
#9944=EDGE_CURVE('',#7604,#7606,#4866,.T.);
#9945=EDGE_CURVE('',#7607,#7606,#421,.T.);
#9946=EDGE_CURVE('',#7605,#7607,#4867,.T.);
#9947=EDGE_CURVE('',#7608,#7604,#422,.T.);
#9948=EDGE_CURVE('',#7609,#7608,#4868,.T.);
#9949=EDGE_CURVE('',#7606,#7609,#423,.T.);
#9950=EDGE_CURVE('',#7610,#7611,#424,.T.);
#9951=EDGE_CURVE('',#7610,#7612,#4869,.T.);
#9952=EDGE_CURVE('',#7613,#7612,#425,.T.);
#9953=EDGE_CURVE('',#7611,#7613,#4870,.T.);
#9954=EDGE_CURVE('',#7614,#7610,#426,.T.);
#9955=EDGE_CURVE('',#7615,#7614,#4871,.T.);
#9956=EDGE_CURVE('',#7612,#7615,#427,.T.);
#9957=EDGE_CURVE('',#7616,#7617,#428,.T.);
#9958=EDGE_CURVE('',#7616,#7618,#4872,.T.);
#9959=EDGE_CURVE('',#7619,#7618,#429,.T.);
#9960=EDGE_CURVE('',#7617,#7619,#4873,.T.);
#9961=EDGE_CURVE('',#7620,#7616,#430,.T.);
#9962=EDGE_CURVE('',#7621,#7620,#4874,.T.);
#9963=EDGE_CURVE('',#7618,#7621,#431,.T.);
#9964=EDGE_CURVE('',#7617,#7584,#1620,.T.);
#9965=EDGE_CURVE('',#7619,#7585,#1621,.T.);
#9966=EDGE_CURVE('',#7581,#7548,#1622,.T.);
#9967=EDGE_CURVE('',#7583,#7549,#1623,.T.);
#9968=EDGE_CURVE('',#7547,#7555,#1624,.T.);
#9969=EDGE_CURVE('',#7545,#7554,#1625,.T.);
#9970=EDGE_CURVE('',#7551,#7542,#1626,.T.);
#9971=EDGE_CURVE('',#7553,#7543,#1627,.T.);
#9972=EDGE_CURVE('',#7541,#7561,#1628,.T.);
#9973=EDGE_CURVE('',#7539,#7560,#1629,.T.);
#9974=EDGE_CURVE('',#7557,#7536,#1630,.T.);
#9975=EDGE_CURVE('',#7559,#7537,#1631,.T.);
#9976=EDGE_CURVE('',#7535,#7567,#1632,.T.);
#9977=EDGE_CURVE('',#7533,#7566,#1633,.T.);
#9978=EDGE_CURVE('',#7563,#7530,#1634,.T.);
#9979=EDGE_CURVE('',#7565,#7531,#1635,.T.);
#9980=EDGE_CURVE('',#7529,#7573,#1636,.T.);
#9981=EDGE_CURVE('',#7527,#7572,#1637,.T.);
#9982=EDGE_CURVE('',#7569,#7524,#1638,.T.);
#9983=EDGE_CURVE('',#7571,#7525,#1639,.T.);
#9984=EDGE_CURVE('',#7523,#7579,#1640,.T.);
#9985=EDGE_CURVE('',#7521,#7578,#1641,.T.);
#9986=EDGE_CURVE('',#7575,#7518,#1642,.T.);
#9987=EDGE_CURVE('',#7577,#7519,#1643,.T.);
#9988=EDGE_CURVE('',#7515,#7512,#1644,.T.);
#9989=EDGE_CURVE('',#7517,#7513,#1645,.T.);
#9990=EDGE_CURVE('',#7511,#7591,#1646,.T.);
#9991=EDGE_CURVE('',#7509,#7590,#1647,.T.);
#9992=EDGE_CURVE('',#7587,#7506,#1648,.T.);
#9993=EDGE_CURVE('',#7589,#7507,#1649,.T.);
#9994=EDGE_CURVE('',#7505,#7597,#1650,.T.);
#9995=EDGE_CURVE('',#7503,#7596,#1651,.T.);
#9996=EDGE_CURVE('',#7593,#7500,#1652,.T.);
#9997=EDGE_CURVE('',#7595,#7501,#1653,.T.);
#9998=EDGE_CURVE('',#7499,#7603,#1654,.T.);
#9999=EDGE_CURVE('',#7497,#7602,#1655,.T.);
#10000=EDGE_CURVE('',#7599,#7494,#1656,.T.);
#10001=EDGE_CURVE('',#7601,#7495,#1657,.T.);
#10002=EDGE_CURVE('',#7493,#7609,#1658,.T.);
#10003=EDGE_CURVE('',#7491,#7608,#1659,.T.);
#10004=EDGE_CURVE('',#7605,#7488,#1660,.T.);
#10005=EDGE_CURVE('',#7607,#7489,#1661,.T.);
#10006=EDGE_CURVE('',#7487,#7615,#1662,.T.);
#10007=EDGE_CURVE('',#7485,#7614,#1663,.T.);
#10008=EDGE_CURVE('',#7611,#7482,#1664,.T.);
#10009=EDGE_CURVE('',#7613,#7483,#1665,.T.);
#10010=EDGE_CURVE('',#7481,#7621,#1666,.T.);
#10011=EDGE_CURVE('',#7479,#7620,#1667,.T.);
#10012=EDGE_CURVE('',#7510,#7622,#4875,.T.);
#10013=EDGE_CURVE('',#7622,#7622,#1668,.T.);
#10014=EDGE_CURVE('',#7623,#7623,#1669,.T.);
#10015=EDGE_CURVE('',#7475,#7623,#4876,.T.);
#10016=EDGE_CURVE('',#7477,#7473,#1670,.T.);
#10017=EDGE_CURVE('',#7624,#7624,#1671,.T.);
#10018=EDGE_CURVE('',#7624,#7508,#4877,.T.);
#10019=ORIENTED_EDGE('',*,*,#7625,.T.);
#10020=ORIENTED_EDGE('',*,*,#7626,.T.);
#10021=ORIENTED_EDGE('',*,*,#7627,.T.);
#10022=ORIENTED_EDGE('',*,*,#7628,.T.);
#10023=ORIENTED_EDGE('',*,*,#7629,.T.);
#10024=ORIENTED_EDGE('',*,*,#7630,.T.);
#10025=ORIENTED_EDGE('',*,*,#7628,.F.);
#10026=ORIENTED_EDGE('',*,*,#7631,.F.);
#10027=ORIENTED_EDGE('',*,*,#7632,.F.);
#10028=ORIENTED_EDGE('',*,*,#7633,.F.);
#10029=ORIENTED_EDGE('',*,*,#7634,.T.);
#10030=ORIENTED_EDGE('',*,*,#7627,.F.);
#10031=ORIENTED_EDGE('',*,*,#7635,.T.);
#10032=ORIENTED_EDGE('',*,*,#7636,.F.);
#10033=ORIENTED_EDGE('',*,*,#7637,.F.);
#10034=ORIENTED_EDGE('',*,*,#7638,.F.);
#10035=ORIENTED_EDGE('',*,*,#7631,.T.);
#10036=ORIENTED_EDGE('',*,*,#7626,.F.);
#10037=ORIENTED_EDGE('',*,*,#7639,.F.);
#10038=ORIENTED_EDGE('',*,*,#7640,.F.);
#10039=ORIENTED_EDGE('',*,*,#7635,.F.);
#10040=ORIENTED_EDGE('',*,*,#7636,.T.);
#10041=ORIENTED_EDGE('',*,*,#7640,.T.);
#10042=ORIENTED_EDGE('',*,*,#7641,.T.);
#10043=ORIENTED_EDGE('',*,*,#7642,.T.);
#10044=ORIENTED_EDGE('',*,*,#7643,.T.);
#10045=ORIENTED_EDGE('',*,*,#7644,.T.);
#10046=ORIENTED_EDGE('',*,*,#7644,.F.);
#10047=ORIENTED_EDGE('',*,*,#7645,.T.);
#10048=ORIENTED_EDGE('',*,*,#7646,.T.);
#10049=ORIENTED_EDGE('',*,*,#7647,.F.);
#10050=ORIENTED_EDGE('',*,*,#7637,.T.);
#10051=ORIENTED_EDGE('',*,*,#7648,.T.);
#10052=ORIENTED_EDGE('',*,*,#7649,.T.);
#10053=ORIENTED_EDGE('',*,*,#7650,.T.);
#10054=ORIENTED_EDGE('',*,*,#7651,.T.);
#10055=ORIENTED_EDGE('',*,*,#7652,.T.);
#10056=ORIENTED_EDGE('',*,*,#7653,.T.);
#10057=ORIENTED_EDGE('',*,*,#7649,.F.);
#10058=ORIENTED_EDGE('',*,*,#7654,.F.);
#10059=ORIENTED_EDGE('',*,*,#7655,.F.);
#10060=ORIENTED_EDGE('',*,*,#7656,.F.);
#10061=ORIENTED_EDGE('',*,*,#7648,.F.);
#10062=ORIENTED_EDGE('',*,*,#7657,.F.);
#10063=ORIENTED_EDGE('',*,*,#7658,.F.);
#10064=ORIENTED_EDGE('',*,*,#7659,.F.);
#10065=ORIENTED_EDGE('',*,*,#7654,.T.);
#10066=ORIENTED_EDGE('',*,*,#7653,.F.);
#10067=ORIENTED_EDGE('',*,*,#7660,.T.);
#10068=ORIENTED_EDGE('',*,*,#7661,.T.);
#10069=ORIENTED_EDGE('',*,*,#7662,.F.);
#10070=ORIENTED_EDGE('',*,*,#7657,.T.);
#10071=ORIENTED_EDGE('',*,*,#7663,.T.);
#10072=ORIENTED_EDGE('',*,*,#7664,.T.);
#10073=ORIENTED_EDGE('',*,*,#7665,.T.);
#10074=ORIENTED_EDGE('',*,*,#7666,.T.);
#10075=ORIENTED_EDGE('',*,*,#7667,.T.);
#10076=ORIENTED_EDGE('',*,*,#7668,.T.);
#10077=ORIENTED_EDGE('',*,*,#7665,.F.);
#10078=ORIENTED_EDGE('',*,*,#7669,.T.);
#10079=ORIENTED_EDGE('',*,*,#7670,.T.);
#10080=ORIENTED_EDGE('',*,*,#7671,.F.);
#10081=ORIENTED_EDGE('',*,*,#7672,.T.);
#10082=ORIENTED_EDGE('',*,*,#7664,.F.);
#10083=ORIENTED_EDGE('',*,*,#7673,.F.);
#10084=ORIENTED_EDGE('',*,*,#7674,.F.);
#10085=ORIENTED_EDGE('',*,*,#7669,.F.);
#10086=ORIENTED_EDGE('',*,*,#7663,.F.);
#10087=ORIENTED_EDGE('',*,*,#7675,.T.);
#10088=ORIENTED_EDGE('',*,*,#7676,.T.);
#10089=ORIENTED_EDGE('',*,*,#7677,.T.);
#10090=ORIENTED_EDGE('',*,*,#7673,.T.);
#10091=ORIENTED_EDGE('',*,*,#7678,.T.);
#10092=ORIENTED_EDGE('',*,*,#7679,.T.);
#10093=ORIENTED_EDGE('',*,*,#7680,.T.);
#10094=ORIENTED_EDGE('',*,*,#7681,.T.);
#10095=ORIENTED_EDGE('',*,*,#7682,.T.);
#10096=ORIENTED_EDGE('',*,*,#7683,.T.);
#10097=ORIENTED_EDGE('',*,*,#7680,.F.);
#10098=ORIENTED_EDGE('',*,*,#7684,.T.);
#10099=ORIENTED_EDGE('',*,*,#7685,.F.);
#10100=ORIENTED_EDGE('',*,*,#7686,.T.);
#10101=ORIENTED_EDGE('',*,*,#7687,.T.);
#10102=ORIENTED_EDGE('',*,*,#7688,.T.);
#10103=ORIENTED_EDGE('',*,*,#7679,.F.);
#10104=ORIENTED_EDGE('',*,*,#7689,.F.);
#10105=ORIENTED_EDGE('',*,*,#7690,.F.);
#10106=ORIENTED_EDGE('',*,*,#7684,.F.);
#10107=ORIENTED_EDGE('',*,*,#7678,.F.);
#10108=ORIENTED_EDGE('',*,*,#7691,.F.);
#10109=ORIENTED_EDGE('',*,*,#7692,.F.);
#10110=ORIENTED_EDGE('',*,*,#7693,.T.);
#10111=ORIENTED_EDGE('',*,*,#7694,.F.);
#10112=ORIENTED_EDGE('',*,*,#7689,.T.);
#10113=ORIENTED_EDGE('',*,*,#7685,.T.);
#10114=ORIENTED_EDGE('',*,*,#7690,.T.);
#10115=ORIENTED_EDGE('',*,*,#7694,.T.);
#10116=ORIENTED_EDGE('',*,*,#7695,.T.);
#10117=ORIENTED_EDGE('',*,*,#7696,.T.);
#10118=ORIENTED_EDGE('',*,*,#7697,.T.);
#10119=ORIENTED_EDGE('',*,*,#7698,.T.);
#10120=ORIENTED_EDGE('',*,*,#7699,.T.);
#10121=ORIENTED_EDGE('',*,*,#7700,.T.);
#10122=ORIENTED_EDGE('',*,*,#7699,.F.);
#10123=ORIENTED_EDGE('',*,*,#7698,.F.);
#10124=ORIENTED_EDGE('',*,*,#7701,.T.);
#10125=ORIENTED_EDGE('',*,*,#7702,.F.);
#10126=ORIENTED_EDGE('',*,*,#7701,.F.);
#10127=ORIENTED_EDGE('',*,*,#7703,.F.);
#10128=ORIENTED_EDGE('',*,*,#7700,.F.);
#10129=ORIENTED_EDGE('',*,*,#7702,.T.);
#10130=ORIENTED_EDGE('',*,*,#7704,.T.);
#10131=ORIENTED_EDGE('',*,*,#7705,.T.);
#10132=ORIENTED_EDGE('',*,*,#7704,.F.);
#10133=ORIENTED_EDGE('',*,*,#7705,.F.);
#10134=ORIENTED_EDGE('',*,*,#7706,.T.);
#10135=ORIENTED_EDGE('',*,*,#7707,.T.);
#10136=ORIENTED_EDGE('',*,*,#7706,.F.);
#10137=ORIENTED_EDGE('',*,*,#7708,.F.);
#10138=ORIENTED_EDGE('',*,*,#7709,.T.);
#10139=ORIENTED_EDGE('',*,*,#7710,.T.);
#10140=ORIENTED_EDGE('',*,*,#7711,.T.);
#10141=ORIENTED_EDGE('',*,*,#7709,.F.);
#10142=ORIENTED_EDGE('',*,*,#7708,.T.);
#10143=ORIENTED_EDGE('',*,*,#7710,.F.);
#10144=ORIENTED_EDGE('',*,*,#7711,.F.);
#10145=ORIENTED_EDGE('',*,*,#7712,.T.);
#10146=ORIENTED_EDGE('',*,*,#7713,.F.);
#10147=ORIENTED_EDGE('',*,*,#7714,.F.);
#10148=ORIENTED_EDGE('',*,*,#7712,.F.);
#10149=ORIENTED_EDGE('',*,*,#7715,.T.);
#10150=ORIENTED_EDGE('',*,*,#7716,.T.);
#10151=ORIENTED_EDGE('',*,*,#7717,.T.);
#10152=ORIENTED_EDGE('',*,*,#7718,.T.);
#10153=ORIENTED_EDGE('',*,*,#7719,.T.);
#10154=ORIENTED_EDGE('',*,*,#7720,.T.);
#10155=ORIENTED_EDGE('',*,*,#7719,.F.);
#10156=ORIENTED_EDGE('',*,*,#7721,.F.);
#10157=ORIENTED_EDGE('',*,*,#7722,.T.);
#10158=ORIENTED_EDGE('',*,*,#7723,.F.);
#10159=ORIENTED_EDGE('',*,*,#7718,.F.);
#10160=ORIENTED_EDGE('',*,*,#7724,.F.);
#10161=ORIENTED_EDGE('',*,*,#7725,.F.);
#10162=ORIENTED_EDGE('',*,*,#7726,.F.);
#10163=ORIENTED_EDGE('',*,*,#7727,.F.);
#10164=ORIENTED_EDGE('',*,*,#7721,.T.);
#10165=ORIENTED_EDGE('',*,*,#7717,.F.);
#10166=ORIENTED_EDGE('',*,*,#7728,.T.);
#10167=ORIENTED_EDGE('',*,*,#7729,.T.);
#10168=ORIENTED_EDGE('',*,*,#7730,.T.);
#10169=ORIENTED_EDGE('',*,*,#7724,.T.);
#10170=ORIENTED_EDGE('',*,*,#7731,.T.);
#10171=ORIENTED_EDGE('',*,*,#7732,.T.);
#10172=ORIENTED_EDGE('',*,*,#7733,.T.);
#10173=ORIENTED_EDGE('',*,*,#7734,.T.);
#10174=ORIENTED_EDGE('',*,*,#7735,.T.);
#10175=ORIENTED_EDGE('',*,*,#7736,.T.);
#10176=ORIENTED_EDGE('',*,*,#7733,.F.);
#10177=ORIENTED_EDGE('',*,*,#7737,.T.);
#10178=ORIENTED_EDGE('',*,*,#7738,.F.);
#10179=ORIENTED_EDGE('',*,*,#7739,.T.);
#10180=ORIENTED_EDGE('',*,*,#7740,.T.);
#10181=ORIENTED_EDGE('',*,*,#7732,.F.);
#10182=ORIENTED_EDGE('',*,*,#7741,.F.);
#10183=ORIENTED_EDGE('',*,*,#7742,.F.);
#10184=ORIENTED_EDGE('',*,*,#7737,.F.);
#10185=ORIENTED_EDGE('',*,*,#7731,.F.);
#10186=ORIENTED_EDGE('',*,*,#7743,.T.);
#10187=ORIENTED_EDGE('',*,*,#7744,.T.);
#10188=ORIENTED_EDGE('',*,*,#7745,.F.);
#10189=ORIENTED_EDGE('',*,*,#7741,.T.);
#10190=ORIENTED_EDGE('',*,*,#7746,.T.);
#10191=ORIENTED_EDGE('',*,*,#7747,.T.);
#10192=ORIENTED_EDGE('',*,*,#7729,.F.);
#10193=ORIENTED_EDGE('',*,*,#7748,.T.);
#10194=ORIENTED_EDGE('',*,*,#7749,.T.);
#10195=ORIENTED_EDGE('',*,*,#7750,.T.);
#10196=ORIENTED_EDGE('',*,*,#7746,.F.);
#10197=ORIENTED_EDGE('',*,*,#7751,.T.);
#10198=ORIENTED_EDGE('',*,*,#7745,.T.);
#10199=ORIENTED_EDGE('',*,*,#7752,.T.);
#10200=ORIENTED_EDGE('',*,*,#7749,.F.);
#10201=ORIENTED_EDGE('',*,*,#7753,.T.);
#10202=ORIENTED_EDGE('',*,*,#7736,.F.);
#10203=ORIENTED_EDGE('',*,*,#7754,.T.);
#10204=ORIENTED_EDGE('',*,*,#7755,.T.);
#10205=ORIENTED_EDGE('',*,*,#7756,.F.);
#10206=ORIENTED_EDGE('',*,*,#7757,.T.);
#10207=ORIENTED_EDGE('',*,*,#7743,.F.);
#10208=ORIENTED_EDGE('',*,*,#7735,.F.);
#10209=ORIENTED_EDGE('',*,*,#7758,.F.);
#10210=ORIENTED_EDGE('',*,*,#7759,.F.);
#10211=ORIENTED_EDGE('',*,*,#7754,.F.);
#10212=ORIENTED_EDGE('',*,*,#7753,.F.);
#10213=ORIENTED_EDGE('',*,*,#7760,.T.);
#10214=ORIENTED_EDGE('',*,*,#7761,.F.);
#10215=ORIENTED_EDGE('',*,*,#7742,.T.);
#10216=ORIENTED_EDGE('',*,*,#7751,.F.);
#10217=ORIENTED_EDGE('',*,*,#7762,.F.);
#10218=ORIENTED_EDGE('',*,*,#7763,.F.);
#10219=ORIENTED_EDGE('',*,*,#7760,.F.);
#10220=ORIENTED_EDGE('',*,*,#7748,.F.);
#10221=ORIENTED_EDGE('',*,*,#7764,.T.);
#10222=ORIENTED_EDGE('',*,*,#7765,.F.);
#10223=ORIENTED_EDGE('',*,*,#7762,.T.);
#10224=ORIENTED_EDGE('',*,*,#7716,.F.);
#10225=ORIENTED_EDGE('',*,*,#7766,.F.);
#10226=ORIENTED_EDGE('',*,*,#7764,.F.);
#10227=ORIENTED_EDGE('',*,*,#7728,.F.);
#10228=ORIENTED_EDGE('',*,*,#7767,.T.);
#10229=ORIENTED_EDGE('',*,*,#7768,.T.);
#10230=ORIENTED_EDGE('',*,*,#7769,.T.);
#10231=ORIENTED_EDGE('',*,*,#7770,.T.);
#10232=ORIENTED_EDGE('',*,*,#7771,.T.);
#10233=ORIENTED_EDGE('',*,*,#7772,.T.);
#10234=ORIENTED_EDGE('',*,*,#7769,.F.);
#10235=ORIENTED_EDGE('',*,*,#7773,.T.);
#10236=ORIENTED_EDGE('',*,*,#7774,.T.);
#10237=ORIENTED_EDGE('',*,*,#7775,.T.);
#10238=ORIENTED_EDGE('',*,*,#7771,.F.);
#10239=ORIENTED_EDGE('',*,*,#7776,.T.);
#10240=ORIENTED_EDGE('',*,*,#7777,.T.);
#10241=ORIENTED_EDGE('',*,*,#7778,.T.);
#10242=ORIENTED_EDGE('',*,*,#7774,.F.);
#10243=ORIENTED_EDGE('',*,*,#7779,.T.);
#10244=ORIENTED_EDGE('',*,*,#7780,.T.);
#10245=ORIENTED_EDGE('',*,*,#7781,.T.);
#10246=ORIENTED_EDGE('',*,*,#7777,.F.);
#10247=ORIENTED_EDGE('',*,*,#7782,.T.);
#10248=ORIENTED_EDGE('',*,*,#7744,.F.);
#10249=ORIENTED_EDGE('',*,*,#7757,.F.);
#10250=ORIENTED_EDGE('',*,*,#7770,.F.);
#10251=ORIENTED_EDGE('',*,*,#7783,.F.);
#10252=ORIENTED_EDGE('',*,*,#7752,.F.);
#10253=ORIENTED_EDGE('',*,*,#7783,.T.);
#10254=ORIENTED_EDGE('',*,*,#7772,.F.);
#10255=ORIENTED_EDGE('',*,*,#7784,.F.);
#10256=ORIENTED_EDGE('',*,*,#7750,.F.);
#10257=ORIENTED_EDGE('',*,*,#7784,.T.);
#10258=ORIENTED_EDGE('',*,*,#7775,.F.);
#10259=ORIENTED_EDGE('',*,*,#7785,.F.);
#10260=ORIENTED_EDGE('',*,*,#7747,.F.);
#10261=ORIENTED_EDGE('',*,*,#7785,.T.);
#10262=ORIENTED_EDGE('',*,*,#7778,.F.);
#10263=ORIENTED_EDGE('',*,*,#7786,.F.);
#10264=ORIENTED_EDGE('',*,*,#7730,.F.);
#10265=ORIENTED_EDGE('',*,*,#7786,.T.);
#10266=ORIENTED_EDGE('',*,*,#7781,.F.);
#10267=ORIENTED_EDGE('',*,*,#7725,.T.);
#10268=ORIENTED_EDGE('',*,*,#7780,.F.);
#10269=ORIENTED_EDGE('',*,*,#7787,.T.);
#10270=ORIENTED_EDGE('',*,*,#7788,.T.);
#10271=ORIENTED_EDGE('',*,*,#7726,.T.);
#10272=ORIENTED_EDGE('',*,*,#7789,.T.);
#10273=ORIENTED_EDGE('',*,*,#7790,.T.);
#10274=ORIENTED_EDGE('',*,*,#7788,.F.);
#10275=ORIENTED_EDGE('',*,*,#7791,.T.);
#10276=ORIENTED_EDGE('',*,*,#7647,.T.);
#10277=ORIENTED_EDGE('',*,*,#7789,.F.);
#10278=ORIENTED_EDGE('',*,*,#7792,.T.);
#10279=ORIENTED_EDGE('',*,*,#7793,.T.);
#10280=ORIENTED_EDGE('',*,*,#7794,.T.);
#10281=ORIENTED_EDGE('',*,*,#7795,.T.);
#10282=ORIENTED_EDGE('',*,*,#7638,.T.);
#10283=ORIENTED_EDGE('',*,*,#7793,.F.);
#10284=ORIENTED_EDGE('',*,*,#7796,.T.);
#10285=ORIENTED_EDGE('',*,*,#7797,.T.);
#10286=ORIENTED_EDGE('',*,*,#7632,.T.);
#10287=ORIENTED_EDGE('',*,*,#7795,.F.);
#10288=ORIENTED_EDGE('',*,*,#7798,.T.);
#10289=ORIENTED_EDGE('',*,*,#7799,.T.);
#10290=ORIENTED_EDGE('',*,*,#7797,.F.);
#10291=ORIENTED_EDGE('',*,*,#7800,.T.);
#10292=ORIENTED_EDGE('',*,*,#7662,.T.);
#10293=ORIENTED_EDGE('',*,*,#7798,.F.);
#10294=ORIENTED_EDGE('',*,*,#7801,.T.);
#10295=ORIENTED_EDGE('',*,*,#7802,.T.);
#10296=ORIENTED_EDGE('',*,*,#7803,.T.);
#10297=ORIENTED_EDGE('',*,*,#7804,.T.);
#10298=ORIENTED_EDGE('',*,*,#7658,.T.);
#10299=ORIENTED_EDGE('',*,*,#7802,.F.);
#10300=ORIENTED_EDGE('',*,*,#7805,.T.);
#10301=ORIENTED_EDGE('',*,*,#7806,.T.);
#10302=ORIENTED_EDGE('',*,*,#7804,.F.);
#10303=ORIENTED_EDGE('',*,*,#7807,.T.);
#10304=ORIENTED_EDGE('',*,*,#7808,.T.);
#10305=ORIENTED_EDGE('',*,*,#7809,.T.);
#10306=ORIENTED_EDGE('',*,*,#7805,.F.);
#10307=ORIENTED_EDGE('',*,*,#7810,.T.);
#10308=ORIENTED_EDGE('',*,*,#7811,.T.);
#10309=ORIENTED_EDGE('',*,*,#7812,.T.);
#10310=ORIENTED_EDGE('',*,*,#7808,.F.);
#10311=ORIENTED_EDGE('',*,*,#7813,.T.);
#10312=ORIENTED_EDGE('',*,*,#7671,.T.);
#10313=ORIENTED_EDGE('',*,*,#7811,.F.);
#10314=ORIENTED_EDGE('',*,*,#7814,.T.);
#10315=ORIENTED_EDGE('',*,*,#7815,.T.);
#10316=ORIENTED_EDGE('',*,*,#7816,.T.);
#10317=ORIENTED_EDGE('',*,*,#7817,.T.);
#10318=ORIENTED_EDGE('',*,*,#7818,.T.);
#10319=ORIENTED_EDGE('',*,*,#7815,.F.);
#10320=ORIENTED_EDGE('',*,*,#7819,.T.);
#10321=ORIENTED_EDGE('',*,*,#7820,.T.);
#10322=ORIENTED_EDGE('',*,*,#7817,.F.);
#10323=ORIENTED_EDGE('',*,*,#7821,.T.);
#10324=ORIENTED_EDGE('',*,*,#7822,.T.);
#10325=ORIENTED_EDGE('',*,*,#7819,.F.);
#10326=ORIENTED_EDGE('',*,*,#7823,.T.);
#10327=ORIENTED_EDGE('',*,*,#7824,.T.);
#10328=ORIENTED_EDGE('',*,*,#7825,.T.);
#10329=ORIENTED_EDGE('',*,*,#7826,.T.);
#10330=ORIENTED_EDGE('',*,*,#7692,.T.);
#10331=ORIENTED_EDGE('',*,*,#7824,.F.);
#10332=ORIENTED_EDGE('',*,*,#7827,.T.);
#10333=ORIENTED_EDGE('',*,*,#7828,.T.);
#10334=ORIENTED_EDGE('',*,*,#7829,.T.);
#10335=ORIENTED_EDGE('',*,*,#7826,.F.);
#10336=ORIENTED_EDGE('',*,*,#7830,.T.);
#10337=ORIENTED_EDGE('',*,*,#7831,.T.);
#10338=ORIENTED_EDGE('',*,*,#7828,.F.);
#10339=ORIENTED_EDGE('',*,*,#7832,.T.);
#10340=ORIENTED_EDGE('',*,*,#7767,.F.);
#10341=ORIENTED_EDGE('',*,*,#7756,.T.);
#10342=ORIENTED_EDGE('',*,*,#7830,.F.);
#10343=ORIENTED_EDGE('',*,*,#7833,.T.);
#10344=ORIENTED_EDGE('',*,*,#7768,.F.);
#10345=ORIENTED_EDGE('',*,*,#7833,.F.);
#10346=ORIENTED_EDGE('',*,*,#7832,.F.);
#10347=ORIENTED_EDGE('',*,*,#7827,.F.);
#10348=ORIENTED_EDGE('',*,*,#7825,.F.);
#10349=ORIENTED_EDGE('',*,*,#7823,.F.);
#10350=ORIENTED_EDGE('',*,*,#7821,.F.);
#10351=ORIENTED_EDGE('',*,*,#7816,.F.);
#10352=ORIENTED_EDGE('',*,*,#7814,.F.);
#10353=ORIENTED_EDGE('',*,*,#7813,.F.);
#10354=ORIENTED_EDGE('',*,*,#7810,.F.);
#10355=ORIENTED_EDGE('',*,*,#7807,.F.);
#10356=ORIENTED_EDGE('',*,*,#7803,.F.);
#10357=ORIENTED_EDGE('',*,*,#7801,.F.);
#10358=ORIENTED_EDGE('',*,*,#7800,.F.);
#10359=ORIENTED_EDGE('',*,*,#7796,.F.);
#10360=ORIENTED_EDGE('',*,*,#7794,.F.);
#10361=ORIENTED_EDGE('',*,*,#7792,.F.);
#10362=ORIENTED_EDGE('',*,*,#7791,.F.);
#10363=ORIENTED_EDGE('',*,*,#7787,.F.);
#10364=ORIENTED_EDGE('',*,*,#7782,.F.);
#10365=ORIENTED_EDGE('',*,*,#7779,.F.);
#10366=ORIENTED_EDGE('',*,*,#7776,.F.);
#10367=ORIENTED_EDGE('',*,*,#7773,.F.);
#10368=ORIENTED_EDGE('',*,*,#7834,.F.);
#10369=ORIENTED_EDGE('',*,*,#7835,.T.);
#10370=ORIENTED_EDGE('',*,*,#7713,.T.);
#10371=ORIENTED_EDGE('',*,*,#7714,.T.);
#10372=ORIENTED_EDGE('',*,*,#7835,.F.);
#10373=ORIENTED_EDGE('',*,*,#7836,.T.);
#10374=ORIENTED_EDGE('',*,*,#7837,.F.);
#10375=ORIENTED_EDGE('',*,*,#7838,.T.);
#10376=ORIENTED_EDGE('',*,*,#7839,.F.);
#10377=ORIENTED_EDGE('',*,*,#7840,.F.);
#10378=ORIENTED_EDGE('',*,*,#7838,.F.);
#10379=ORIENTED_EDGE('',*,*,#7836,.F.);
#10380=ORIENTED_EDGE('',*,*,#7841,.T.);
#10381=ORIENTED_EDGE('',*,*,#7842,.T.);
#10382=ORIENTED_EDGE('',*,*,#7837,.T.);
#10383=ORIENTED_EDGE('',*,*,#7842,.F.);
#10384=ORIENTED_EDGE('',*,*,#7703,.T.);
#10385=ORIENTED_EDGE('',*,*,#7843,.T.);
#10386=ORIENTED_EDGE('',*,*,#7841,.F.);
#10387=ORIENTED_EDGE('',*,*,#7843,.F.);
#10388=ORIENTED_EDGE('',*,*,#7840,.T.);
#10389=ORIENTED_EDGE('',*,*,#7844,.T.);
#10390=ORIENTED_EDGE('',*,*,#7834,.T.);
#10391=ORIENTED_EDGE('',*,*,#7844,.F.);
#10392=ORIENTED_EDGE('',*,*,#7839,.T.);
#10393=ORIENTED_EDGE('',*,*,#7707,.F.);
#10394=ORIENTED_EDGE('',*,*,#7715,.F.);
#10395=ORIENTED_EDGE('',*,*,#7845,.T.);
#10396=ORIENTED_EDGE('',*,*,#7846,.T.);
#10397=ORIENTED_EDGE('',*,*,#7847,.T.);
#10398=ORIENTED_EDGE('',*,*,#7766,.T.);
#10399=ORIENTED_EDGE('',*,*,#7625,.F.);
#10400=ORIENTED_EDGE('',*,*,#7848,.T.);
#10401=ORIENTED_EDGE('',*,*,#7849,.T.);
#10402=ORIENTED_EDGE('',*,*,#7850,.T.);
#10403=ORIENTED_EDGE('',*,*,#7641,.F.);
#10404=ORIENTED_EDGE('',*,*,#7639,.T.);
#10405=ORIENTED_EDGE('',*,*,#7851,.T.);
#10406=ORIENTED_EDGE('',*,*,#7852,.T.);
#10407=ORIENTED_EDGE('',*,*,#7677,.F.);
#10408=ORIENTED_EDGE('',*,*,#7853,.T.);
#10409=ORIENTED_EDGE('',*,*,#7854,.T.);
#10410=ORIENTED_EDGE('',*,*,#7855,.T.);
#10411=ORIENTED_EDGE('',*,*,#7851,.F.);
#10412=ORIENTED_EDGE('',*,*,#7856,.T.);
#10413=ORIENTED_EDGE('',*,*,#7857,.T.);
#10414=ORIENTED_EDGE('',*,*,#7858,.T.);
#10415=ORIENTED_EDGE('',*,*,#7854,.F.);
#10416=ORIENTED_EDGE('',*,*,#7859,.T.);
#10417=ORIENTED_EDGE('',*,*,#7650,.F.);
#10418=ORIENTED_EDGE('',*,*,#7656,.T.);
#10419=ORIENTED_EDGE('',*,*,#7857,.F.);
#10420=ORIENTED_EDGE('',*,*,#7860,.T.);
#10421=ORIENTED_EDGE('',*,*,#7861,.T.);
#10422=ORIENTED_EDGE('',*,*,#7668,.F.);
#10423=ORIENTED_EDGE('',*,*,#7862,.T.);
#10424=ORIENTED_EDGE('',*,*,#7863,.T.);
#10425=ORIENTED_EDGE('',*,*,#7864,.T.);
#10426=ORIENTED_EDGE('',*,*,#7675,.F.);
#10427=ORIENTED_EDGE('',*,*,#7865,.T.);
#10428=ORIENTED_EDGE('',*,*,#7866,.T.);
#10429=ORIENTED_EDGE('',*,*,#7863,.F.);
#10430=ORIENTED_EDGE('',*,*,#7867,.T.);
#10431=ORIENTED_EDGE('',*,*,#7681,.F.);
#10432=ORIENTED_EDGE('',*,*,#7688,.F.);
#10433=ORIENTED_EDGE('',*,*,#7868,.T.);
#10434=ORIENTED_EDGE('',*,*,#7865,.F.);
#10435=ORIENTED_EDGE('',*,*,#7869,.T.);
#10436=ORIENTED_EDGE('',*,*,#7630,.F.);
#10437=ORIENTED_EDGE('',*,*,#7870,.T.);
#10438=ORIENTED_EDGE('',*,*,#7871,.T.);
#10439=ORIENTED_EDGE('',*,*,#7872,.T.);
#10440=ORIENTED_EDGE('',*,*,#7848,.F.);
#10441=ORIENTED_EDGE('',*,*,#7873,.T.);
#10442=ORIENTED_EDGE('',*,*,#7874,.T.);
#10443=ORIENTED_EDGE('',*,*,#7871,.F.);
#10444=ORIENTED_EDGE('',*,*,#7875,.T.);
#10445=ORIENTED_EDGE('',*,*,#7651,.F.);
#10446=ORIENTED_EDGE('',*,*,#7861,.F.);
#10447=ORIENTED_EDGE('',*,*,#7876,.T.);
#10448=ORIENTED_EDGE('',*,*,#7873,.F.);
#10449=ORIENTED_EDGE('',*,*,#7877,.T.);
#10450=ORIENTED_EDGE('',*,*,#7697,.F.);
#10451=ORIENTED_EDGE('',*,*,#7878,.T.);
#10452=ORIENTED_EDGE('',*,*,#7879,.T.);
#10453=ORIENTED_EDGE('',*,*,#7880,.T.);
#10454=ORIENTED_EDGE('',*,*,#7686,.F.);
#10455=ORIENTED_EDGE('',*,*,#7881,.T.);
#10456=ORIENTED_EDGE('',*,*,#7882,.T.);
#10457=ORIENTED_EDGE('',*,*,#7879,.F.);
#10458=ORIENTED_EDGE('',*,*,#7883,.T.);
#10459=ORIENTED_EDGE('',*,*,#7734,.F.);
#10460=ORIENTED_EDGE('',*,*,#7740,.F.);
#10461=ORIENTED_EDGE('',*,*,#7884,.T.);
#10462=ORIENTED_EDGE('',*,*,#7881,.F.);
#10463=ORIENTED_EDGE('',*,*,#7758,.T.);
#10464=ORIENTED_EDGE('',*,*,#7720,.F.);
#10465=ORIENTED_EDGE('',*,*,#7723,.T.);
#10466=ORIENTED_EDGE('',*,*,#7885,.T.);
#10467=ORIENTED_EDGE('',*,*,#7886,.T.);
#10468=ORIENTED_EDGE('',*,*,#7845,.F.);
#10469=ORIENTED_EDGE('',*,*,#7887,.T.);
#10470=ORIENTED_EDGE('',*,*,#7888,.T.);
#10471=ORIENTED_EDGE('',*,*,#7885,.F.);
#10472=ORIENTED_EDGE('',*,*,#7889,.T.);
#10473=ORIENTED_EDGE('',*,*,#7642,.F.);
#10474=ORIENTED_EDGE('',*,*,#7850,.F.);
#10475=ORIENTED_EDGE('',*,*,#7890,.T.);
#10476=ORIENTED_EDGE('',*,*,#7887,.F.);
#10477=ORIENTED_EDGE('',*,*,#7891,.T.);
#10478=ORIENTED_EDGE('',*,*,#7892,.T.);
#10479=ORIENTED_EDGE('',*,*,#7765,.T.);
#10480=ORIENTED_EDGE('',*,*,#7847,.F.);
#10481=ORIENTED_EDGE('',*,*,#7893,.T.);
#10482=ORIENTED_EDGE('',*,*,#7894,.T.);
#10483=ORIENTED_EDGE('',*,*,#7763,.T.);
#10484=ORIENTED_EDGE('',*,*,#7892,.F.);
#10485=ORIENTED_EDGE('',*,*,#7895,.T.);
#10486=ORIENTED_EDGE('',*,*,#7738,.T.);
#10487=ORIENTED_EDGE('',*,*,#7761,.T.);
#10488=ORIENTED_EDGE('',*,*,#7894,.F.);
#10489=ORIENTED_EDGE('',*,*,#7896,.T.);
#10490=ORIENTED_EDGE('',*,*,#7883,.F.);
#10491=ORIENTED_EDGE('',*,*,#7897,.F.);
#10492=ORIENTED_EDGE('',*,*,#7898,.F.);
#10493=ORIENTED_EDGE('',*,*,#7759,.T.);
#10494=ORIENTED_EDGE('',*,*,#7696,.F.);
#10495=ORIENTED_EDGE('',*,*,#7899,.F.);
#10496=ORIENTED_EDGE('',*,*,#7897,.T.);
#10497=ORIENTED_EDGE('',*,*,#7878,.F.);
#10498=ORIENTED_EDGE('',*,*,#7682,.F.);
#10499=ORIENTED_EDGE('',*,*,#7869,.F.);
#10500=ORIENTED_EDGE('',*,*,#7900,.F.);
#10501=ORIENTED_EDGE('',*,*,#7901,.F.);
#10502=ORIENTED_EDGE('',*,*,#7867,.F.);
#10503=ORIENTED_EDGE('',*,*,#7902,.F.);
#10504=ORIENTED_EDGE('',*,*,#7903,.F.);
#10505=ORIENTED_EDGE('',*,*,#7900,.T.);
#10506=ORIENTED_EDGE('',*,*,#7667,.F.);
#10507=ORIENTED_EDGE('',*,*,#7904,.F.);
#10508=ORIENTED_EDGE('',*,*,#7902,.T.);
#10509=ORIENTED_EDGE('',*,*,#7862,.F.);
#10510=ORIENTED_EDGE('',*,*,#7676,.F.);
#10511=ORIENTED_EDGE('',*,*,#7864,.F.);
#10512=ORIENTED_EDGE('',*,*,#7866,.F.);
#10513=ORIENTED_EDGE('',*,*,#7868,.F.);
#10514=ORIENTED_EDGE('',*,*,#7687,.F.);
#10515=ORIENTED_EDGE('',*,*,#7880,.F.);
#10516=ORIENTED_EDGE('',*,*,#7882,.F.);
#10517=ORIENTED_EDGE('',*,*,#7884,.F.);
#10518=ORIENTED_EDGE('',*,*,#7739,.F.);
#10519=ORIENTED_EDGE('',*,*,#7896,.F.);
#10520=ORIENTED_EDGE('',*,*,#7895,.F.);
#10521=ORIENTED_EDGE('',*,*,#7893,.F.);
#10522=ORIENTED_EDGE('',*,*,#7846,.F.);
#10523=ORIENTED_EDGE('',*,*,#7886,.F.);
#10524=ORIENTED_EDGE('',*,*,#7888,.F.);
#10525=ORIENTED_EDGE('',*,*,#7890,.F.);
#10526=ORIENTED_EDGE('',*,*,#7849,.F.);
#10527=ORIENTED_EDGE('',*,*,#7872,.F.);
#10528=ORIENTED_EDGE('',*,*,#7874,.F.);
#10529=ORIENTED_EDGE('',*,*,#7876,.F.);
#10530=ORIENTED_EDGE('',*,*,#7860,.F.);
#10531=ORIENTED_EDGE('',*,*,#7859,.F.);
#10532=ORIENTED_EDGE('',*,*,#7856,.F.);
#10533=ORIENTED_EDGE('',*,*,#7853,.F.);
#10534=ORIENTED_EDGE('',*,*,#7812,.F.);
#10535=ORIENTED_EDGE('',*,*,#7670,.F.);
#10536=ORIENTED_EDGE('',*,*,#7905,.T.);
#10537=ORIENTED_EDGE('',*,*,#7906,.T.);
#10538=ORIENTED_EDGE('',*,*,#7809,.F.);
#10539=ORIENTED_EDGE('',*,*,#7906,.F.);
#10540=ORIENTED_EDGE('',*,*,#7907,.T.);
#10541=ORIENTED_EDGE('',*,*,#7908,.T.);
#10542=ORIENTED_EDGE('',*,*,#7806,.F.);
#10543=ORIENTED_EDGE('',*,*,#7908,.F.);
#10544=ORIENTED_EDGE('',*,*,#7909,.T.);
#10545=ORIENTED_EDGE('',*,*,#7659,.T.);
#10546=ORIENTED_EDGE('',*,*,#7683,.F.);
#10547=ORIENTED_EDGE('',*,*,#7901,.T.);
#10548=ORIENTED_EDGE('',*,*,#7910,.T.);
#10549=ORIENTED_EDGE('',*,*,#7822,.F.);
#10550=ORIENTED_EDGE('',*,*,#7691,.T.);
#10551=ORIENTED_EDGE('',*,*,#7820,.F.);
#10552=ORIENTED_EDGE('',*,*,#7910,.F.);
#10553=ORIENTED_EDGE('',*,*,#7903,.T.);
#10554=ORIENTED_EDGE('',*,*,#7911,.T.);
#10555=ORIENTED_EDGE('',*,*,#7666,.F.);
#10556=ORIENTED_EDGE('',*,*,#7672,.F.);
#10557=ORIENTED_EDGE('',*,*,#7818,.F.);
#10558=ORIENTED_EDGE('',*,*,#7911,.F.);
#10559=ORIENTED_EDGE('',*,*,#7904,.T.);
#10560=ORIENTED_EDGE('',*,*,#7799,.F.);
#10561=ORIENTED_EDGE('',*,*,#7661,.F.);
#10562=ORIENTED_EDGE('',*,*,#7912,.T.);
#10563=ORIENTED_EDGE('',*,*,#7633,.T.);
#10564=ORIENTED_EDGE('',*,*,#7831,.F.);
#10565=ORIENTED_EDGE('',*,*,#7755,.F.);
#10566=ORIENTED_EDGE('',*,*,#7898,.T.);
#10567=ORIENTED_EDGE('',*,*,#7913,.T.);
#10568=ORIENTED_EDGE('',*,*,#7695,.F.);
#10569=ORIENTED_EDGE('',*,*,#7693,.F.);
#10570=ORIENTED_EDGE('',*,*,#7829,.F.);
#10571=ORIENTED_EDGE('',*,*,#7913,.F.);
#10572=ORIENTED_EDGE('',*,*,#7899,.T.);
#10573=ORIENTED_EDGE('',*,*,#7790,.F.);
#10574=ORIENTED_EDGE('',*,*,#7646,.F.);
#10575=ORIENTED_EDGE('',*,*,#7914,.T.);
#10576=ORIENTED_EDGE('',*,*,#7727,.T.);
#10577=ORIENTED_EDGE('',*,*,#7858,.F.);
#10578=ORIENTED_EDGE('',*,*,#7655,.T.);
#10579=ORIENTED_EDGE('',*,*,#7909,.F.);
#10580=ORIENTED_EDGE('',*,*,#7915,.T.);
#10581=ORIENTED_EDGE('',*,*,#7855,.F.);
#10582=ORIENTED_EDGE('',*,*,#7915,.F.);
#10583=ORIENTED_EDGE('',*,*,#7907,.F.);
#10584=ORIENTED_EDGE('',*,*,#7916,.F.);
#10585=ORIENTED_EDGE('',*,*,#7852,.F.);
#10586=ORIENTED_EDGE('',*,*,#7916,.T.);
#10587=ORIENTED_EDGE('',*,*,#7905,.F.);
#10588=ORIENTED_EDGE('',*,*,#7674,.T.);
#10589=ORIENTED_EDGE('',*,*,#7643,.F.);
#10590=ORIENTED_EDGE('',*,*,#7891,.F.);
#10591=ORIENTED_EDGE('',*,*,#7917,.F.);
#10592=ORIENTED_EDGE('',*,*,#7645,.F.);
#10593=ORIENTED_EDGE('',*,*,#7889,.F.);
#10594=ORIENTED_EDGE('',*,*,#7722,.F.);
#10595=ORIENTED_EDGE('',*,*,#7914,.F.);
#10596=ORIENTED_EDGE('',*,*,#7917,.T.);
#10597=ORIENTED_EDGE('',*,*,#7652,.F.);
#10598=ORIENTED_EDGE('',*,*,#7877,.F.);
#10599=ORIENTED_EDGE('',*,*,#7918,.F.);
#10600=ORIENTED_EDGE('',*,*,#7660,.F.);
#10601=ORIENTED_EDGE('',*,*,#7629,.F.);
#10602=ORIENTED_EDGE('',*,*,#7634,.F.);
#10603=ORIENTED_EDGE('',*,*,#7919,.T.);
#10604=ORIENTED_EDGE('',*,*,#7870,.F.);
#10605=ORIENTED_EDGE('',*,*,#7875,.F.);
#10606=ORIENTED_EDGE('',*,*,#7919,.F.);
#10607=ORIENTED_EDGE('',*,*,#7912,.F.);
#10608=ORIENTED_EDGE('',*,*,#7918,.T.);
#10609=ORIENTED_EDGE('',*,*,#7920,.F.);
#10610=ORIENTED_EDGE('',*,*,#7921,.F.);
#10611=ORIENTED_EDGE('',*,*,#7922,.F.);
#10612=ORIENTED_EDGE('',*,*,#7923,.T.);
#10613=ORIENTED_EDGE('',*,*,#7920,.T.);
#10614=ORIENTED_EDGE('',*,*,#7923,.F.);
#10615=ORIENTED_EDGE('',*,*,#7924,.F.);
#10616=ORIENTED_EDGE('',*,*,#7925,.F.);
#10617=ORIENTED_EDGE('',*,*,#7926,.F.);
#10618=ORIENTED_EDGE('',*,*,#7927,.T.);
#10619=ORIENTED_EDGE('',*,*,#7922,.T.);
#10620=ORIENTED_EDGE('',*,*,#7927,.F.);
#10621=ORIENTED_EDGE('',*,*,#7928,.F.);
#10622=ORIENTED_EDGE('',*,*,#7929,.F.);
#10623=ORIENTED_EDGE('',*,*,#7930,.F.);
#10624=ORIENTED_EDGE('',*,*,#7931,.F.);
#10625=ORIENTED_EDGE('',*,*,#7932,.T.);
#10626=ORIENTED_EDGE('',*,*,#7933,.F.);
#10627=ORIENTED_EDGE('',*,*,#7932,.F.);
#10628=ORIENTED_EDGE('',*,*,#7931,.T.);
#10629=ORIENTED_EDGE('',*,*,#7934,.F.);
#10630=ORIENTED_EDGE('',*,*,#7935,.F.);
#10631=ORIENTED_EDGE('',*,*,#7936,.F.);
#10632=ORIENTED_EDGE('',*,*,#7937,.T.);
#10633=ORIENTED_EDGE('',*,*,#7934,.T.);
#10634=ORIENTED_EDGE('',*,*,#7937,.F.);
#10635=ORIENTED_EDGE('',*,*,#7938,.F.);
#10636=ORIENTED_EDGE('',*,*,#7925,.T.);
#10637=ORIENTED_EDGE('',*,*,#7939,.F.);
#10638=ORIENTED_EDGE('',*,*,#7929,.T.);
#10639=ORIENTED_EDGE('',*,*,#7921,.T.);
#10640=ORIENTED_EDGE('',*,*,#7940,.T.);
#10641=ORIENTED_EDGE('',*,*,#7941,.F.);
#10642=ORIENTED_EDGE('',*,*,#7942,.F.);
#10643=ORIENTED_EDGE('',*,*,#7943,.F.);
#10644=ORIENTED_EDGE('',*,*,#7940,.F.);
#10645=ORIENTED_EDGE('',*,*,#7944,.F.);
#10646=ORIENTED_EDGE('',*,*,#7945,.F.);
#10647=ORIENTED_EDGE('',*,*,#7933,.T.);
#10648=ORIENTED_EDGE('',*,*,#7946,.T.);
#10649=ORIENTED_EDGE('',*,*,#7947,.F.);
#10650=ORIENTED_EDGE('',*,*,#7948,.T.);
#10651=ORIENTED_EDGE('',*,*,#7949,.F.);
#10652=ORIENTED_EDGE('',*,*,#7945,.T.);
#10653=ORIENTED_EDGE('',*,*,#7950,.F.);
#10654=ORIENTED_EDGE('',*,*,#7946,.F.);
#10655=ORIENTED_EDGE('',*,*,#7951,.F.);
#10656=ORIENTED_EDGE('',*,*,#7948,.F.);
#10657=ORIENTED_EDGE('',*,*,#7952,.F.);
#10658=ORIENTED_EDGE('',*,*,#7953,.F.);
#10659=ORIENTED_EDGE('',*,*,#7954,.T.);
#10660=ORIENTED_EDGE('',*,*,#7952,.T.);
#10661=ORIENTED_EDGE('',*,*,#7954,.F.);
#10662=ORIENTED_EDGE('',*,*,#7955,.F.);
#10663=ORIENTED_EDGE('',*,*,#7956,.T.);
#10664=ORIENTED_EDGE('',*,*,#7953,.T.);
#10665=ORIENTED_EDGE('',*,*,#7956,.F.);
#10666=ORIENTED_EDGE('',*,*,#7957,.F.);
#10667=ORIENTED_EDGE('',*,*,#7955,.T.);
#10668=ORIENTED_EDGE('',*,*,#7958,.F.);
#10669=ORIENTED_EDGE('',*,*,#7959,.T.);
#10670=ORIENTED_EDGE('',*,*,#7957,.T.);
#10671=ORIENTED_EDGE('',*,*,#7959,.F.);
#10672=ORIENTED_EDGE('',*,*,#7960,.F.);
#10673=ORIENTED_EDGE('',*,*,#7961,.T.);
#10674=ORIENTED_EDGE('',*,*,#7942,.T.);
#10675=ORIENTED_EDGE('',*,*,#7941,.T.);
#10676=ORIENTED_EDGE('',*,*,#7962,.T.);
#10677=ORIENTED_EDGE('',*,*,#7958,.T.);
#10678=ORIENTED_EDGE('',*,*,#7962,.F.);
#10679=ORIENTED_EDGE('',*,*,#7943,.T.);
#10680=ORIENTED_EDGE('',*,*,#7961,.F.);
#10681=ORIENTED_EDGE('',*,*,#7935,.T.);
#10682=ORIENTED_EDGE('',*,*,#7936,.T.);
#10683=ORIENTED_EDGE('',*,*,#7963,.F.);
#10684=ORIENTED_EDGE('',*,*,#7964,.T.);
#10685=ORIENTED_EDGE('',*,*,#7960,.T.);
#10686=ORIENTED_EDGE('',*,*,#7964,.F.);
#10687=ORIENTED_EDGE('',*,*,#7963,.T.);
#10688=ORIENTED_EDGE('',*,*,#7965,.F.);
#10689=ORIENTED_EDGE('',*,*,#7965,.T.);
#10690=ORIENTED_EDGE('',*,*,#7966,.T.);
#10691=ORIENTED_EDGE('',*,*,#7967,.F.);
#10692=ORIENTED_EDGE('',*,*,#7966,.F.);
#10693=ORIENTED_EDGE('',*,*,#7967,.T.);
#10694=ORIENTED_EDGE('',*,*,#7968,.T.);
#10695=ORIENTED_EDGE('',*,*,#7930,.T.);
#10696=ORIENTED_EDGE('',*,*,#7939,.T.);
#10697=ORIENTED_EDGE('',*,*,#7928,.T.);
#10698=ORIENTED_EDGE('',*,*,#7969,.T.);
#10699=ORIENTED_EDGE('',*,*,#7970,.F.);
#10700=ORIENTED_EDGE('',*,*,#7969,.F.);
#10701=ORIENTED_EDGE('',*,*,#7926,.T.);
#10702=ORIENTED_EDGE('',*,*,#7938,.T.);
#10703=ORIENTED_EDGE('',*,*,#7924,.T.);
#10704=ORIENTED_EDGE('',*,*,#7968,.F.);
#10705=ORIENTED_EDGE('',*,*,#7949,.T.);
#10706=ORIENTED_EDGE('',*,*,#7951,.T.);
#10707=ORIENTED_EDGE('',*,*,#7947,.T.);
#10708=ORIENTED_EDGE('',*,*,#7950,.T.);
#10709=ORIENTED_EDGE('',*,*,#7944,.T.);
#10710=ORIENTED_EDGE('',*,*,#7970,.T.);
#10711=ORIENTED_EDGE('',*,*,#7971,.T.);
#10712=ORIENTED_EDGE('',*,*,#7972,.T.);
#10713=ORIENTED_EDGE('',*,*,#7973,.T.);
#10714=ORIENTED_EDGE('',*,*,#7974,.T.);
#10715=ORIENTED_EDGE('',*,*,#7972,.F.);
#10716=ORIENTED_EDGE('',*,*,#7973,.F.);
#10717=ORIENTED_EDGE('',*,*,#7974,.F.);
#10718=ORIENTED_EDGE('',*,*,#7975,.T.);
#10719=ORIENTED_EDGE('',*,*,#7976,.F.);
#10720=ORIENTED_EDGE('',*,*,#7977,.F.);
#10721=ORIENTED_EDGE('',*,*,#7975,.F.);
#10722=ORIENTED_EDGE('',*,*,#7971,.F.);
#10723=ORIENTED_EDGE('',*,*,#7976,.T.);
#10724=ORIENTED_EDGE('',*,*,#7977,.T.);
#10725=ORIENTED_EDGE('',*,*,#7978,.T.);
#10726=ORIENTED_EDGE('',*,*,#7979,.T.);
#10727=ORIENTED_EDGE('',*,*,#7980,.T.);
#10728=ORIENTED_EDGE('',*,*,#7978,.F.);
#10729=ORIENTED_EDGE('',*,*,#7979,.F.);
#10730=ORIENTED_EDGE('',*,*,#7980,.F.);
#10731=ORIENTED_EDGE('',*,*,#7981,.T.);
#10732=ORIENTED_EDGE('',*,*,#7982,.F.);
#10733=ORIENTED_EDGE('',*,*,#7983,.F.);
#10734=ORIENTED_EDGE('',*,*,#7981,.F.);
#10735=ORIENTED_EDGE('',*,*,#7982,.T.);
#10736=ORIENTED_EDGE('',*,*,#7983,.T.);
#10737=ORIENTED_EDGE('',*,*,#7984,.T.);
#10738=ORIENTED_EDGE('',*,*,#7985,.T.);
#10739=ORIENTED_EDGE('',*,*,#7986,.T.);
#10740=ORIENTED_EDGE('',*,*,#7984,.F.);
#10741=ORIENTED_EDGE('',*,*,#7985,.F.);
#10742=ORIENTED_EDGE('',*,*,#7986,.F.);
#10743=ORIENTED_EDGE('',*,*,#7987,.T.);
#10744=ORIENTED_EDGE('',*,*,#7988,.F.);
#10745=ORIENTED_EDGE('',*,*,#7989,.F.);
#10746=ORIENTED_EDGE('',*,*,#7987,.F.);
#10747=ORIENTED_EDGE('',*,*,#7988,.T.);
#10748=ORIENTED_EDGE('',*,*,#7989,.T.);
#10749=ORIENTED_EDGE('',*,*,#7990,.T.);
#10750=ORIENTED_EDGE('',*,*,#7991,.T.);
#10751=ORIENTED_EDGE('',*,*,#7990,.F.);
#10752=ORIENTED_EDGE('',*,*,#7991,.F.);
#10753=ORIENTED_EDGE('',*,*,#7992,.T.);
#10754=ORIENTED_EDGE('',*,*,#7993,.T.);
#10755=ORIENTED_EDGE('',*,*,#7994,.T.);
#10756=ORIENTED_EDGE('',*,*,#7995,.T.);
#10757=ORIENTED_EDGE('',*,*,#7996,.T.);
#10758=ORIENTED_EDGE('',*,*,#7997,.T.);
#10759=ORIENTED_EDGE('',*,*,#7995,.F.);
#10760=ORIENTED_EDGE('',*,*,#7998,.T.);
#10761=ORIENTED_EDGE('',*,*,#7999,.T.);
#10762=ORIENTED_EDGE('',*,*,#8000,.T.);
#10763=ORIENTED_EDGE('',*,*,#8001,.T.);
#10764=ORIENTED_EDGE('',*,*,#8002,.T.);
#10765=ORIENTED_EDGE('',*,*,#7994,.F.);
#10766=ORIENTED_EDGE('',*,*,#8003,.F.);
#10767=ORIENTED_EDGE('',*,*,#8004,.F.);
#10768=ORIENTED_EDGE('',*,*,#8005,.F.);
#10769=ORIENTED_EDGE('',*,*,#8006,.F.);
#10770=ORIENTED_EDGE('',*,*,#8007,.F.);
#10771=ORIENTED_EDGE('',*,*,#8008,.F.);
#10772=ORIENTED_EDGE('',*,*,#8009,.F.);
#10773=ORIENTED_EDGE('',*,*,#7998,.F.);
#10774=ORIENTED_EDGE('',*,*,#7993,.F.);
#10775=ORIENTED_EDGE('',*,*,#8010,.T.);
#10776=ORIENTED_EDGE('',*,*,#8011,.F.);
#10777=ORIENTED_EDGE('',*,*,#8003,.T.);
#10778=ORIENTED_EDGE('',*,*,#7997,.F.);
#10779=ORIENTED_EDGE('',*,*,#8012,.T.);
#10780=ORIENTED_EDGE('',*,*,#8013,.T.);
#10781=ORIENTED_EDGE('',*,*,#8014,.T.);
#10782=ORIENTED_EDGE('',*,*,#8015,.T.);
#10783=ORIENTED_EDGE('',*,*,#8016,.T.);
#10784=ORIENTED_EDGE('',*,*,#7996,.F.);
#10785=ORIENTED_EDGE('',*,*,#8002,.F.);
#10786=ORIENTED_EDGE('',*,*,#8017,.F.);
#10787=ORIENTED_EDGE('',*,*,#8012,.F.);
#10788=ORIENTED_EDGE('',*,*,#7992,.F.);
#10789=ORIENTED_EDGE('',*,*,#8016,.F.);
#10790=ORIENTED_EDGE('',*,*,#8018,.F.);
#10791=ORIENTED_EDGE('',*,*,#8019,.F.);
#10792=ORIENTED_EDGE('',*,*,#8020,.F.);
#10793=ORIENTED_EDGE('',*,*,#8021,.F.);
#10794=ORIENTED_EDGE('',*,*,#8022,.F.);
#10795=ORIENTED_EDGE('',*,*,#8023,.F.);
#10796=ORIENTED_EDGE('',*,*,#8010,.F.);
#10797=ORIENTED_EDGE('',*,*,#8013,.F.);
#10798=ORIENTED_EDGE('',*,*,#8017,.T.);
#10799=ORIENTED_EDGE('',*,*,#8001,.F.);
#10800=ORIENTED_EDGE('',*,*,#8024,.T.);
#10801=ORIENTED_EDGE('',*,*,#8025,.F.);
#10802=ORIENTED_EDGE('',*,*,#8026,.T.);
#10803=ORIENTED_EDGE('',*,*,#8000,.F.);
#10804=ORIENTED_EDGE('',*,*,#8027,.F.);
#10805=ORIENTED_EDGE('',*,*,#8028,.F.);
#10806=ORIENTED_EDGE('',*,*,#8029,.F.);
#10807=ORIENTED_EDGE('',*,*,#8030,.F.);
#10808=ORIENTED_EDGE('',*,*,#8031,.F.);
#10809=ORIENTED_EDGE('',*,*,#8032,.F.);
#10810=ORIENTED_EDGE('',*,*,#8024,.F.);
#10811=ORIENTED_EDGE('',*,*,#8033,.T.);
#10812=ORIENTED_EDGE('',*,*,#8034,.T.);
#10813=ORIENTED_EDGE('',*,*,#8020,.T.);
#10814=ORIENTED_EDGE('',*,*,#8035,.T.);
#10815=ORIENTED_EDGE('',*,*,#8036,.T.);
#10816=ORIENTED_EDGE('',*,*,#8037,.T.);
#10817=ORIENTED_EDGE('',*,*,#8037,.F.);
#10818=ORIENTED_EDGE('',*,*,#8038,.T.);
#10819=ORIENTED_EDGE('',*,*,#8039,.T.);
#10820=ORIENTED_EDGE('',*,*,#8040,.T.);
#10821=ORIENTED_EDGE('',*,*,#8041,.T.);
#10822=ORIENTED_EDGE('',*,*,#8042,.T.);
#10823=ORIENTED_EDGE('',*,*,#8036,.F.);
#10824=ORIENTED_EDGE('',*,*,#8043,.F.);
#10825=ORIENTED_EDGE('',*,*,#8044,.F.);
#10826=ORIENTED_EDGE('',*,*,#8038,.F.);
#10827=ORIENTED_EDGE('',*,*,#8035,.F.);
#10828=ORIENTED_EDGE('',*,*,#8019,.T.);
#10829=ORIENTED_EDGE('',*,*,#8045,.T.);
#10830=ORIENTED_EDGE('',*,*,#8046,.T.);
#10831=ORIENTED_EDGE('',*,*,#8047,.T.);
#10832=ORIENTED_EDGE('',*,*,#8043,.T.);
#10833=ORIENTED_EDGE('',*,*,#8034,.F.);
#10834=ORIENTED_EDGE('',*,*,#8048,.T.);
#10835=ORIENTED_EDGE('',*,*,#8049,.F.);
#10836=ORIENTED_EDGE('',*,*,#8021,.T.);
#10837=ORIENTED_EDGE('',*,*,#8033,.F.);
#10838=ORIENTED_EDGE('',*,*,#8042,.F.);
#10839=ORIENTED_EDGE('',*,*,#8050,.F.);
#10840=ORIENTED_EDGE('',*,*,#8051,.F.);
#10841=ORIENTED_EDGE('',*,*,#8052,.F.);
#10842=ORIENTED_EDGE('',*,*,#8053,.F.);
#10843=ORIENTED_EDGE('',*,*,#8054,.F.);
#10844=ORIENTED_EDGE('',*,*,#8055,.F.);
#10845=ORIENTED_EDGE('',*,*,#8048,.F.);
#10846=ORIENTED_EDGE('',*,*,#8056,.T.);
#10847=ORIENTED_EDGE('',*,*,#8057,.T.);
#10848=ORIENTED_EDGE('',*,*,#8052,.T.);
#10849=ORIENTED_EDGE('',*,*,#8058,.T.);
#10850=ORIENTED_EDGE('',*,*,#8059,.T.);
#10851=ORIENTED_EDGE('',*,*,#8060,.T.);
#10852=ORIENTED_EDGE('',*,*,#8060,.F.);
#10853=ORIENTED_EDGE('',*,*,#8061,.T.);
#10854=ORIENTED_EDGE('',*,*,#8062,.T.);
#10855=ORIENTED_EDGE('',*,*,#8063,.T.);
#10856=ORIENTED_EDGE('',*,*,#8064,.T.);
#10857=ORIENTED_EDGE('',*,*,#8065,.T.);
#10858=ORIENTED_EDGE('',*,*,#8059,.F.);
#10859=ORIENTED_EDGE('',*,*,#8066,.F.);
#10860=ORIENTED_EDGE('',*,*,#8067,.F.);
#10861=ORIENTED_EDGE('',*,*,#8061,.F.);
#10862=ORIENTED_EDGE('',*,*,#8058,.F.);
#10863=ORIENTED_EDGE('',*,*,#8051,.T.);
#10864=ORIENTED_EDGE('',*,*,#8068,.T.);
#10865=ORIENTED_EDGE('',*,*,#8069,.T.);
#10866=ORIENTED_EDGE('',*,*,#8070,.T.);
#10867=ORIENTED_EDGE('',*,*,#8066,.T.);
#10868=ORIENTED_EDGE('',*,*,#8070,.F.);
#10869=ORIENTED_EDGE('',*,*,#8071,.T.);
#10870=ORIENTED_EDGE('',*,*,#8072,.F.);
#10871=ORIENTED_EDGE('',*,*,#8073,.T.);
#10872=ORIENTED_EDGE('',*,*,#8062,.F.);
#10873=ORIENTED_EDGE('',*,*,#8067,.T.);
#10874=ORIENTED_EDGE('',*,*,#8040,.F.);
#10875=ORIENTED_EDGE('',*,*,#8074,.F.);
#10876=ORIENTED_EDGE('',*,*,#8075,.F.);
#10877=ORIENTED_EDGE('',*,*,#8076,.F.);
#10878=ORIENTED_EDGE('',*,*,#8077,.F.);
#10879=ORIENTED_EDGE('',*,*,#8071,.F.);
#10880=ORIENTED_EDGE('',*,*,#8069,.F.);
#10881=ORIENTED_EDGE('',*,*,#8078,.F.);
#10882=ORIENTED_EDGE('',*,*,#8056,.F.);
#10883=ORIENTED_EDGE('',*,*,#8065,.F.);
#10884=ORIENTED_EDGE('',*,*,#8079,.F.);
#10885=ORIENTED_EDGE('',*,*,#8080,.F.);
#10886=ORIENTED_EDGE('',*,*,#8081,.F.);
#10887=ORIENTED_EDGE('',*,*,#8082,.F.);
#10888=ORIENTED_EDGE('',*,*,#8083,.F.);
#10889=ORIENTED_EDGE('',*,*,#8084,.F.);
#10890=ORIENTED_EDGE('',*,*,#8085,.F.);
#10891=ORIENTED_EDGE('',*,*,#8064,.F.);
#10892=ORIENTED_EDGE('',*,*,#8086,.T.);
#10893=ORIENTED_EDGE('',*,*,#8087,.F.);
#10894=ORIENTED_EDGE('',*,*,#8079,.T.);
#10895=ORIENTED_EDGE('',*,*,#8063,.F.);
#10896=ORIENTED_EDGE('',*,*,#8073,.F.);
#10897=ORIENTED_EDGE('',*,*,#8088,.F.);
#10898=ORIENTED_EDGE('',*,*,#8089,.F.);
#10899=ORIENTED_EDGE('',*,*,#8090,.F.);
#10900=ORIENTED_EDGE('',*,*,#8091,.F.);
#10901=ORIENTED_EDGE('',*,*,#8092,.F.);
#10902=ORIENTED_EDGE('',*,*,#8086,.F.);
#10903=ORIENTED_EDGE('',*,*,#8007,.T.);
#10904=ORIENTED_EDGE('',*,*,#8093,.T.);
#10905=ORIENTED_EDGE('',*,*,#8081,.T.);
#10906=ORIENTED_EDGE('',*,*,#8094,.T.);
#10907=ORIENTED_EDGE('',*,*,#8095,.T.);
#10908=ORIENTED_EDGE('',*,*,#8096,.T.);
#10909=ORIENTED_EDGE('',*,*,#8094,.F.);
#10910=ORIENTED_EDGE('',*,*,#8080,.T.);
#10911=ORIENTED_EDGE('',*,*,#8087,.T.);
#10912=ORIENTED_EDGE('',*,*,#8092,.T.);
#10913=ORIENTED_EDGE('',*,*,#8097,.T.);
#10914=ORIENTED_EDGE('',*,*,#8098,.T.);
#10915=ORIENTED_EDGE('',*,*,#8093,.F.);
#10916=ORIENTED_EDGE('',*,*,#8006,.T.);
#10917=ORIENTED_EDGE('',*,*,#8099,.F.);
#10918=ORIENTED_EDGE('',*,*,#8082,.T.);
#10919=ORIENTED_EDGE('',*,*,#8096,.F.);
#10920=ORIENTED_EDGE('',*,*,#8100,.T.);
#10921=ORIENTED_EDGE('',*,*,#8101,.T.);
#10922=ORIENTED_EDGE('',*,*,#8028,.T.);
#10923=ORIENTED_EDGE('',*,*,#8102,.T.);
#10924=ORIENTED_EDGE('',*,*,#8008,.T.);
#10925=ORIENTED_EDGE('',*,*,#8101,.F.);
#10926=ORIENTED_EDGE('',*,*,#8103,.T.);
#10927=ORIENTED_EDGE('',*,*,#8097,.F.);
#10928=ORIENTED_EDGE('',*,*,#8091,.T.);
#10929=ORIENTED_EDGE('',*,*,#8104,.T.);
#10930=ORIENTED_EDGE('',*,*,#8029,.T.);
#10931=ORIENTED_EDGE('',*,*,#8095,.F.);
#10932=ORIENTED_EDGE('',*,*,#8098,.F.);
#10933=ORIENTED_EDGE('',*,*,#8103,.F.);
#10934=ORIENTED_EDGE('',*,*,#8100,.F.);
#10935=ORIENTED_EDGE('',*,*,#8054,.T.);
#10936=ORIENTED_EDGE('',*,*,#8105,.T.);
#10937=ORIENTED_EDGE('',*,*,#8084,.T.);
#10938=ORIENTED_EDGE('',*,*,#8106,.T.);
#10939=ORIENTED_EDGE('',*,*,#8107,.T.);
#10940=ORIENTED_EDGE('',*,*,#8108,.T.);
#10941=ORIENTED_EDGE('',*,*,#8106,.F.);
#10942=ORIENTED_EDGE('',*,*,#8083,.T.);
#10943=ORIENTED_EDGE('',*,*,#8099,.T.);
#10944=ORIENTED_EDGE('',*,*,#8005,.T.);
#10945=ORIENTED_EDGE('',*,*,#8109,.F.);
#10946=ORIENTED_EDGE('',*,*,#8110,.T.);
#10947=ORIENTED_EDGE('',*,*,#8057,.F.);
#10948=ORIENTED_EDGE('',*,*,#8085,.T.);
#10949=ORIENTED_EDGE('',*,*,#8105,.F.);
#10950=ORIENTED_EDGE('',*,*,#8053,.T.);
#10951=ORIENTED_EDGE('',*,*,#8004,.T.);
#10952=ORIENTED_EDGE('',*,*,#8011,.T.);
#10953=ORIENTED_EDGE('',*,*,#8023,.T.);
#10954=ORIENTED_EDGE('',*,*,#8111,.T.);
#10955=ORIENTED_EDGE('',*,*,#8112,.T.);
#10956=ORIENTED_EDGE('',*,*,#8109,.T.);
#10957=ORIENTED_EDGE('',*,*,#8107,.F.);
#10958=ORIENTED_EDGE('',*,*,#8110,.F.);
#10959=ORIENTED_EDGE('',*,*,#8112,.F.);
#10960=ORIENTED_EDGE('',*,*,#8113,.F.);
#10961=ORIENTED_EDGE('',*,*,#8114,.F.);
#10962=ORIENTED_EDGE('',*,*,#8115,.F.);
#10963=ORIENTED_EDGE('',*,*,#8116,.F.);
#10964=ORIENTED_EDGE('',*,*,#8117,.F.);
#10965=ORIENTED_EDGE('',*,*,#8118,.F.);
#10966=ORIENTED_EDGE('',*,*,#8119,.F.);
#10967=ORIENTED_EDGE('',*,*,#8108,.F.);
#10968=ORIENTED_EDGE('',*,*,#8113,.T.);
#10969=ORIENTED_EDGE('',*,*,#8111,.F.);
#10970=ORIENTED_EDGE('',*,*,#8022,.T.);
#10971=ORIENTED_EDGE('',*,*,#8049,.T.);
#10972=ORIENTED_EDGE('',*,*,#8055,.T.);
#10973=ORIENTED_EDGE('',*,*,#8104,.F.);
#10974=ORIENTED_EDGE('',*,*,#8090,.T.);
#10975=ORIENTED_EDGE('',*,*,#8120,.F.);
#10976=ORIENTED_EDGE('',*,*,#8030,.T.);
#10977=ORIENTED_EDGE('',*,*,#8047,.F.);
#10978=ORIENTED_EDGE('',*,*,#8121,.T.);
#10979=ORIENTED_EDGE('',*,*,#8122,.T.);
#10980=ORIENTED_EDGE('',*,*,#8074,.T.);
#10981=ORIENTED_EDGE('',*,*,#8039,.F.);
#10982=ORIENTED_EDGE('',*,*,#8044,.T.);
#10983=ORIENTED_EDGE('',*,*,#8122,.F.);
#10984=ORIENTED_EDGE('',*,*,#8123,.T.);
#10985=ORIENTED_EDGE('',*,*,#8124,.F.);
#10986=ORIENTED_EDGE('',*,*,#8075,.T.);
#10987=ORIENTED_EDGE('',*,*,#8014,.F.);
#10988=ORIENTED_EDGE('',*,*,#8026,.F.);
#10989=ORIENTED_EDGE('',*,*,#8125,.F.);
#10990=ORIENTED_EDGE('',*,*,#8126,.F.);
#10991=ORIENTED_EDGE('',*,*,#8123,.F.);
#10992=ORIENTED_EDGE('',*,*,#8121,.F.);
#10993=ORIENTED_EDGE('',*,*,#8046,.F.);
#10994=ORIENTED_EDGE('',*,*,#8127,.F.);
#10995=ORIENTED_EDGE('',*,*,#8128,.T.);
#10996=ORIENTED_EDGE('',*,*,#8129,.T.);
#10997=ORIENTED_EDGE('',*,*,#8130,.T.);
#10998=ORIENTED_EDGE('',*,*,#8131,.T.);
#10999=ORIENTED_EDGE('',*,*,#8132,.T.);
#11000=ORIENTED_EDGE('',*,*,#8130,.F.);
#11001=ORIENTED_EDGE('',*,*,#8133,.F.);
#11002=ORIENTED_EDGE('',*,*,#8134,.F.);
#11003=ORIENTED_EDGE('',*,*,#8135,.T.);
#11004=ORIENTED_EDGE('',*,*,#8128,.F.);
#11005=ORIENTED_EDGE('',*,*,#8129,.F.);
#11006=ORIENTED_EDGE('',*,*,#8135,.F.);
#11007=ORIENTED_EDGE('',*,*,#8131,.F.);
#11008=ORIENTED_EDGE('',*,*,#8132,.F.);
#11009=ORIENTED_EDGE('',*,*,#8136,.T.);
#11010=ORIENTED_EDGE('',*,*,#8137,.F.);
#11011=ORIENTED_EDGE('',*,*,#8136,.F.);
#11012=ORIENTED_EDGE('',*,*,#8138,.T.);
#11013=ORIENTED_EDGE('',*,*,#8139,.T.);
#11014=ORIENTED_EDGE('',*,*,#8133,.T.);
#11015=ORIENTED_EDGE('',*,*,#8134,.T.);
#11016=ORIENTED_EDGE('',*,*,#8139,.F.);
#11017=ORIENTED_EDGE('',*,*,#8140,.F.);
#11018=ORIENTED_EDGE('',*,*,#8138,.F.);
#11019=ORIENTED_EDGE('',*,*,#8141,.T.);
#11020=ORIENTED_EDGE('',*,*,#8142,.T.);
#11021=ORIENTED_EDGE('',*,*,#8143,.T.);
#11022=ORIENTED_EDGE('',*,*,#8144,.T.);
#11023=ORIENTED_EDGE('',*,*,#8142,.F.);
#11024=ORIENTED_EDGE('',*,*,#8145,.F.);
#11025=ORIENTED_EDGE('',*,*,#8141,.F.);
#11026=ORIENTED_EDGE('',*,*,#8143,.F.);
#11027=ORIENTED_EDGE('',*,*,#8144,.F.);
#11028=ORIENTED_EDGE('',*,*,#8146,.T.);
#11029=ORIENTED_EDGE('',*,*,#8140,.T.);
#11030=ORIENTED_EDGE('',*,*,#8146,.F.);
#11031=ORIENTED_EDGE('',*,*,#8119,.T.);
#11032=ORIENTED_EDGE('',*,*,#8147,.T.);
#11033=ORIENTED_EDGE('',*,*,#8148,.T.);
#11034=ORIENTED_EDGE('',*,*,#8147,.F.);
#11035=ORIENTED_EDGE('',*,*,#8148,.F.);
#11036=ORIENTED_EDGE('',*,*,#8149,.T.);
#11037=ORIENTED_EDGE('',*,*,#8145,.T.);
#11038=ORIENTED_EDGE('',*,*,#8149,.F.);
#11039=ORIENTED_EDGE('',*,*,#8114,.T.);
#11040=ORIENTED_EDGE('',*,*,#8150,.T.);
#11041=ORIENTED_EDGE('',*,*,#8151,.T.);
#11042=ORIENTED_EDGE('',*,*,#8150,.F.);
#11043=ORIENTED_EDGE('',*,*,#8152,.F.);
#11044=ORIENTED_EDGE('',*,*,#8153,.F.);
#11045=ORIENTED_EDGE('',*,*,#8154,.T.);
#11046=ORIENTED_EDGE('',*,*,#8151,.F.);
#11047=ORIENTED_EDGE('',*,*,#8154,.F.);
#11048=ORIENTED_EDGE('',*,*,#8155,.T.);
#11049=ORIENTED_EDGE('',*,*,#8156,.T.);
#11050=ORIENTED_EDGE('',*,*,#8152,.T.);
#11051=ORIENTED_EDGE('',*,*,#8153,.T.);
#11052=ORIENTED_EDGE('',*,*,#8156,.F.);
#11053=ORIENTED_EDGE('',*,*,#8157,.F.);
#11054=ORIENTED_EDGE('',*,*,#8155,.F.);
#11055=ORIENTED_EDGE('',*,*,#8118,.T.);
#11056=ORIENTED_EDGE('',*,*,#8158,.T.);
#11057=ORIENTED_EDGE('',*,*,#8159,.T.);
#11058=ORIENTED_EDGE('',*,*,#8158,.F.);
#11059=ORIENTED_EDGE('',*,*,#8160,.F.);
#11060=ORIENTED_EDGE('',*,*,#8161,.F.);
#11061=ORIENTED_EDGE('',*,*,#8162,.T.);
#11062=ORIENTED_EDGE('',*,*,#8159,.F.);
#11063=ORIENTED_EDGE('',*,*,#8162,.F.);
#11064=ORIENTED_EDGE('',*,*,#8163,.T.);
#11065=ORIENTED_EDGE('',*,*,#8164,.T.);
#11066=ORIENTED_EDGE('',*,*,#8160,.T.);
#11067=ORIENTED_EDGE('',*,*,#8161,.T.);
#11068=ORIENTED_EDGE('',*,*,#8164,.F.);
#11069=ORIENTED_EDGE('',*,*,#8165,.F.);
#11070=ORIENTED_EDGE('',*,*,#8163,.F.);
#11071=ORIENTED_EDGE('',*,*,#8115,.T.);
#11072=ORIENTED_EDGE('',*,*,#8166,.T.);
#11073=ORIENTED_EDGE('',*,*,#8167,.T.);
#11074=ORIENTED_EDGE('',*,*,#8166,.F.);
#11075=ORIENTED_EDGE('',*,*,#8168,.F.);
#11076=ORIENTED_EDGE('',*,*,#8169,.T.);
#11077=ORIENTED_EDGE('',*,*,#8167,.F.);
#11078=ORIENTED_EDGE('',*,*,#8169,.F.);
#11079=ORIENTED_EDGE('',*,*,#8117,.T.);
#11080=ORIENTED_EDGE('',*,*,#8170,.T.);
#11081=ORIENTED_EDGE('',*,*,#8171,.T.);
#11082=ORIENTED_EDGE('',*,*,#8170,.F.);
#11083=ORIENTED_EDGE('',*,*,#8172,.F.);
#11084=ORIENTED_EDGE('',*,*,#8173,.T.);
#11085=ORIENTED_EDGE('',*,*,#8171,.F.);
#11086=ORIENTED_EDGE('',*,*,#8173,.F.);
#11087=ORIENTED_EDGE('',*,*,#8116,.T.);
#11088=ORIENTED_EDGE('',*,*,#8174,.T.);
#11089=ORIENTED_EDGE('',*,*,#8175,.T.);
#11090=ORIENTED_EDGE('',*,*,#8174,.F.);
#11091=ORIENTED_EDGE('',*,*,#8176,.F.);
#11092=ORIENTED_EDGE('',*,*,#8177,.T.);
#11093=ORIENTED_EDGE('',*,*,#8175,.F.);
#11094=ORIENTED_EDGE('',*,*,#8177,.F.);
#11095=ORIENTED_EDGE('',*,*,#8178,.T.);
#11096=ORIENTED_EDGE('',*,*,#8179,.T.);
#11097=ORIENTED_EDGE('',*,*,#8180,.T.);
#11098=ORIENTED_EDGE('',*,*,#8179,.F.);
#11099=ORIENTED_EDGE('',*,*,#8181,.F.);
#11100=ORIENTED_EDGE('',*,*,#8182,.F.);
#11101=ORIENTED_EDGE('',*,*,#8183,.F.);
#11102=ORIENTED_EDGE('',*,*,#8184,.F.);
#11103=ORIENTED_EDGE('',*,*,#8185,.F.);
#11104=ORIENTED_EDGE('',*,*,#8186,.F.);
#11105=ORIENTED_EDGE('',*,*,#8187,.F.);
#11106=ORIENTED_EDGE('',*,*,#8188,.F.);
#11107=ORIENTED_EDGE('',*,*,#8189,.F.);
#11108=ORIENTED_EDGE('',*,*,#8178,.F.);
#11109=ORIENTED_EDGE('',*,*,#8180,.F.);
#11110=ORIENTED_EDGE('',*,*,#8190,.T.);
#11111=ORIENTED_EDGE('',*,*,#8165,.T.);
#11112=ORIENTED_EDGE('',*,*,#8190,.F.);
#11113=ORIENTED_EDGE('',*,*,#8185,.T.);
#11114=ORIENTED_EDGE('',*,*,#8191,.T.);
#11115=ORIENTED_EDGE('',*,*,#8192,.T.);
#11116=ORIENTED_EDGE('',*,*,#8191,.F.);
#11117=ORIENTED_EDGE('',*,*,#8192,.F.);
#11118=ORIENTED_EDGE('',*,*,#8193,.T.);
#11119=ORIENTED_EDGE('',*,*,#8157,.T.);
#11120=ORIENTED_EDGE('',*,*,#8193,.F.);
#11121=ORIENTED_EDGE('',*,*,#8189,.T.);
#11122=ORIENTED_EDGE('',*,*,#8194,.T.);
#11123=ORIENTED_EDGE('',*,*,#8137,.T.);
#11124=ORIENTED_EDGE('',*,*,#8194,.F.);
#11125=ORIENTED_EDGE('',*,*,#8125,.T.);
#11126=ORIENTED_EDGE('',*,*,#8025,.T.);
#11127=ORIENTED_EDGE('',*,*,#8032,.T.);
#11128=ORIENTED_EDGE('',*,*,#8195,.T.);
#11129=ORIENTED_EDGE('',*,*,#8181,.T.);
#11130=ORIENTED_EDGE('',*,*,#8196,.T.);
#11131=ORIENTED_EDGE('',*,*,#8195,.F.);
#11132=ORIENTED_EDGE('',*,*,#8031,.T.);
#11133=ORIENTED_EDGE('',*,*,#8120,.T.);
#11134=ORIENTED_EDGE('',*,*,#8089,.T.);
#11135=ORIENTED_EDGE('',*,*,#8197,.F.);
#11136=ORIENTED_EDGE('',*,*,#8182,.T.);
#11137=ORIENTED_EDGE('',*,*,#8088,.T.);
#11138=ORIENTED_EDGE('',*,*,#8072,.T.);
#11139=ORIENTED_EDGE('',*,*,#8077,.T.);
#11140=ORIENTED_EDGE('',*,*,#8198,.T.);
#11141=ORIENTED_EDGE('',*,*,#8183,.T.);
#11142=ORIENTED_EDGE('',*,*,#8197,.T.);
#11143=ORIENTED_EDGE('',*,*,#8196,.F.);
#11144=ORIENTED_EDGE('',*,*,#8184,.T.);
#11145=ORIENTED_EDGE('',*,*,#8198,.F.);
#11146=ORIENTED_EDGE('',*,*,#8076,.T.);
#11147=ORIENTED_EDGE('',*,*,#8124,.T.);
#11148=ORIENTED_EDGE('',*,*,#8126,.T.);
#11149=ORIENTED_EDGE('',*,*,#8186,.T.);
#11150=ORIENTED_EDGE('',*,*,#8199,.T.);
#11151=ORIENTED_EDGE('',*,*,#8176,.T.);
#11152=ORIENTED_EDGE('',*,*,#8199,.F.);
#11153=ORIENTED_EDGE('',*,*,#8188,.T.);
#11154=ORIENTED_EDGE('',*,*,#8200,.T.);
#11155=ORIENTED_EDGE('',*,*,#8172,.T.);
#11156=ORIENTED_EDGE('',*,*,#8200,.F.);
#11157=ORIENTED_EDGE('',*,*,#8187,.T.);
#11158=ORIENTED_EDGE('',*,*,#8201,.T.);
#11159=ORIENTED_EDGE('',*,*,#8168,.T.);
#11160=ORIENTED_EDGE('',*,*,#8201,.F.);
#11161=ORIENTED_EDGE('',*,*,#8041,.F.);
#11162=ORIENTED_EDGE('',*,*,#8078,.T.);
#11163=ORIENTED_EDGE('',*,*,#8068,.F.);
#11164=ORIENTED_EDGE('',*,*,#8050,.T.);
#11165=ORIENTED_EDGE('',*,*,#7999,.F.);
#11166=ORIENTED_EDGE('',*,*,#8009,.T.);
#11167=ORIENTED_EDGE('',*,*,#8102,.F.);
#11168=ORIENTED_EDGE('',*,*,#8027,.T.);
#11169=ORIENTED_EDGE('',*,*,#8015,.F.);
#11170=ORIENTED_EDGE('',*,*,#8127,.T.);
#11171=ORIENTED_EDGE('',*,*,#8045,.F.);
#11172=ORIENTED_EDGE('',*,*,#8018,.T.);
#11173=ORIENTED_EDGE('',*,*,#8202,.F.);
#11174=ORIENTED_EDGE('',*,*,#8203,.F.);
#11175=ORIENTED_EDGE('',*,*,#8204,.T.);
#11176=ORIENTED_EDGE('',*,*,#8202,.T.);
#11177=ORIENTED_EDGE('',*,*,#8204,.F.);
#11178=ORIENTED_EDGE('',*,*,#8205,.F.);
#11179=ORIENTED_EDGE('',*,*,#8206,.T.);
#11180=ORIENTED_EDGE('',*,*,#8203,.T.);
#11181=ORIENTED_EDGE('',*,*,#8206,.F.);
#11182=ORIENTED_EDGE('',*,*,#8207,.F.);
#11183=ORIENTED_EDGE('',*,*,#8208,.T.);
#11184=ORIENTED_EDGE('',*,*,#8205,.T.);
#11185=ORIENTED_EDGE('',*,*,#8208,.F.);
#11186=ORIENTED_EDGE('',*,*,#8207,.T.);
#11187=ORIENTED_EDGE('',*,*,#8209,.F.);
#11188=ORIENTED_EDGE('',*,*,#8210,.T.);
#11189=ORIENTED_EDGE('',*,*,#8211,.T.);
#11190=ORIENTED_EDGE('',*,*,#8212,.T.);
#11191=ORIENTED_EDGE('',*,*,#8213,.F.);
#11192=ORIENTED_EDGE('',*,*,#8214,.T.);
#11193=ORIENTED_EDGE('',*,*,#8209,.T.);
#11194=ORIENTED_EDGE('',*,*,#8215,.T.);
#11195=ORIENTED_EDGE('',*,*,#8216,.F.);
#11196=ORIENTED_EDGE('',*,*,#8217,.T.);
#11197=ORIENTED_EDGE('',*,*,#8218,.F.);
#11198=ORIENTED_EDGE('',*,*,#8219,.F.);
#11199=ORIENTED_EDGE('',*,*,#8220,.F.);
#11200=ORIENTED_EDGE('',*,*,#8221,.F.);
#11201=ORIENTED_EDGE('',*,*,#8222,.T.);
#11202=ORIENTED_EDGE('',*,*,#8216,.T.);
#11203=ORIENTED_EDGE('',*,*,#8223,.F.);
#11204=ORIENTED_EDGE('',*,*,#8224,.F.);
#11205=ORIENTED_EDGE('',*,*,#8225,.F.);
#11206=ORIENTED_EDGE('',*,*,#8226,.F.);
#11207=ORIENTED_EDGE('',*,*,#8227,.T.);
#11208=ORIENTED_EDGE('',*,*,#8223,.T.);
#11209=ORIENTED_EDGE('',*,*,#8219,.T.);
#11210=ORIENTED_EDGE('',*,*,#8228,.F.);
#11211=ORIENTED_EDGE('',*,*,#8229,.F.);
#11212=ORIENTED_EDGE('',*,*,#8215,.F.);
#11213=ORIENTED_EDGE('',*,*,#8212,.F.);
#11214=ORIENTED_EDGE('',*,*,#8230,.F.);
#11215=ORIENTED_EDGE('',*,*,#8231,.F.);
#11216=ORIENTED_EDGE('',*,*,#8232,.T.);
#11217=ORIENTED_EDGE('',*,*,#8233,.F.);
#11218=ORIENTED_EDGE('',*,*,#8234,.T.);
#11219=ORIENTED_EDGE('',*,*,#8235,.T.);
#11220=ORIENTED_EDGE('',*,*,#8236,.F.);
#11221=ORIENTED_EDGE('',*,*,#8237,.T.);
#11222=ORIENTED_EDGE('',*,*,#8238,.F.);
#11223=ORIENTED_EDGE('',*,*,#8239,.T.);
#11224=ORIENTED_EDGE('',*,*,#8240,.T.);
#11225=ORIENTED_EDGE('',*,*,#8231,.T.);
#11226=ORIENTED_EDGE('',*,*,#8241,.F.);
#11227=ORIENTED_EDGE('',*,*,#8242,.T.);
#11228=ORIENTED_EDGE('',*,*,#8243,.T.);
#11229=ORIENTED_EDGE('',*,*,#8244,.F.);
#11230=ORIENTED_EDGE('',*,*,#8210,.F.);
#11231=ORIENTED_EDGE('',*,*,#8214,.F.);
#11232=ORIENTED_EDGE('',*,*,#8245,.F.);
#11233=ORIENTED_EDGE('',*,*,#8246,.F.);
#11234=ORIENTED_EDGE('',*,*,#8217,.F.);
#11235=ORIENTED_EDGE('',*,*,#8222,.F.);
#11236=ORIENTED_EDGE('',*,*,#8247,.F.);
#11237=ORIENTED_EDGE('',*,*,#8248,.F.);
#11238=ORIENTED_EDGE('',*,*,#8235,.F.);
#11239=ORIENTED_EDGE('',*,*,#8249,.F.);
#11240=ORIENTED_EDGE('',*,*,#8250,.F.);
#11241=ORIENTED_EDGE('',*,*,#8251,.F.);
#11242=ORIENTED_EDGE('',*,*,#8252,.F.);
#11243=ORIENTED_EDGE('',*,*,#8253,.F.);
#11244=ORIENTED_EDGE('',*,*,#8239,.F.);
#11245=ORIENTED_EDGE('',*,*,#8220,.T.);
#11246=ORIENTED_EDGE('',*,*,#8227,.F.);
#11247=ORIENTED_EDGE('',*,*,#8254,.F.);
#11248=ORIENTED_EDGE('',*,*,#8251,.T.);
#11249=ORIENTED_EDGE('',*,*,#8255,.F.);
#11250=ORIENTED_EDGE('',*,*,#8256,.F.);
#11251=ORIENTED_EDGE('',*,*,#8257,.F.);
#11252=ORIENTED_EDGE('',*,*,#8232,.F.);
#11253=ORIENTED_EDGE('',*,*,#8240,.F.);
#11254=ORIENTED_EDGE('',*,*,#8253,.T.);
#11255=ORIENTED_EDGE('',*,*,#8218,.T.);
#11256=ORIENTED_EDGE('',*,*,#8246,.T.);
#11257=ORIENTED_EDGE('',*,*,#8258,.F.);
#11258=ORIENTED_EDGE('',*,*,#8259,.F.);
#11259=ORIENTED_EDGE('',*,*,#8228,.T.);
#11260=ORIENTED_EDGE('',*,*,#8260,.F.);
#11261=ORIENTED_EDGE('',*,*,#8261,.F.);
#11262=ORIENTED_EDGE('',*,*,#8242,.F.);
#11263=ORIENTED_EDGE('',*,*,#8224,.T.);
#11264=ORIENTED_EDGE('',*,*,#8257,.T.);
#11265=ORIENTED_EDGE('',*,*,#8252,.T.);
#11266=ORIENTED_EDGE('',*,*,#8238,.T.);
#11267=ORIENTED_EDGE('',*,*,#8262,.F.);
#11268=ORIENTED_EDGE('',*,*,#8263,.F.);
#11269=ORIENTED_EDGE('',*,*,#8264,.F.);
#11270=ORIENTED_EDGE('',*,*,#8265,.F.);
#11271=ORIENTED_EDGE('',*,*,#8266,.T.);
#11272=ORIENTED_EDGE('',*,*,#8236,.T.);
#11273=ORIENTED_EDGE('',*,*,#8230,.T.);
#11274=ORIENTED_EDGE('',*,*,#8211,.F.);
#11275=ORIENTED_EDGE('',*,*,#8244,.T.);
#11276=ORIENTED_EDGE('',*,*,#8267,.T.);
#11277=ORIENTED_EDGE('',*,*,#8268,.F.);
#11278=ORIENTED_EDGE('',*,*,#8269,.F.);
#11279=ORIENTED_EDGE('',*,*,#8270,.F.);
#11280=ORIENTED_EDGE('',*,*,#8271,.F.);
#11281=ORIENTED_EDGE('',*,*,#8213,.T.);
#11282=ORIENTED_EDGE('',*,*,#8229,.T.);
#11283=ORIENTED_EDGE('',*,*,#8272,.F.);
#11284=ORIENTED_EDGE('',*,*,#8245,.T.);
#11285=ORIENTED_EDGE('',*,*,#8261,.T.);
#11286=ORIENTED_EDGE('',*,*,#8273,.T.);
#11287=ORIENTED_EDGE('',*,*,#8249,.T.);
#11288=ORIENTED_EDGE('',*,*,#8274,.T.);
#11289=ORIENTED_EDGE('',*,*,#8247,.T.);
#11290=ORIENTED_EDGE('',*,*,#8221,.T.);
#11291=ORIENTED_EDGE('',*,*,#8256,.T.);
#11292=ORIENTED_EDGE('',*,*,#8275,.F.);
#11293=ORIENTED_EDGE('',*,*,#8276,.F.);
#11294=ORIENTED_EDGE('',*,*,#8277,.F.);
#11295=ORIENTED_EDGE('',*,*,#8267,.F.);
#11296=ORIENTED_EDGE('',*,*,#8260,.T.);
#11297=ORIENTED_EDGE('',*,*,#8241,.T.);
#11298=ORIENTED_EDGE('',*,*,#8278,.F.);
#11299=ORIENTED_EDGE('',*,*,#8279,.F.);
#11300=ORIENTED_EDGE('',*,*,#8280,.F.);
#11301=ORIENTED_EDGE('',*,*,#8281,.F.);
#11302=ORIENTED_EDGE('',*,*,#8275,.T.);
#11303=ORIENTED_EDGE('',*,*,#8255,.T.);
#11304=ORIENTED_EDGE('',*,*,#8250,.T.);
#11305=ORIENTED_EDGE('',*,*,#8273,.F.);
#11306=ORIENTED_EDGE('',*,*,#8225,.T.);
#11307=ORIENTED_EDGE('',*,*,#8266,.F.);
#11308=ORIENTED_EDGE('',*,*,#8282,.F.);
#11309=ORIENTED_EDGE('',*,*,#8283,.F.);
#11310=ORIENTED_EDGE('',*,*,#8226,.T.);
#11311=ORIENTED_EDGE('',*,*,#8283,.T.);
#11312=ORIENTED_EDGE('',*,*,#8284,.F.);
#11313=ORIENTED_EDGE('',*,*,#8285,.F.);
#11314=ORIENTED_EDGE('',*,*,#8286,.F.);
#11315=ORIENTED_EDGE('',*,*,#8287,.F.);
#11316=ORIENTED_EDGE('',*,*,#8233,.T.);
#11317=ORIENTED_EDGE('',*,*,#8248,.T.);
#11318=ORIENTED_EDGE('',*,*,#8254,.T.);
#11319=ORIENTED_EDGE('',*,*,#8288,.T.);
#11320=ORIENTED_EDGE('',*,*,#8289,.T.);
#11321=ORIENTED_EDGE('',*,*,#8276,.T.);
#11322=ORIENTED_EDGE('',*,*,#8281,.T.);
#11323=ORIENTED_EDGE('',*,*,#8290,.F.);
#11324=ORIENTED_EDGE('',*,*,#8284,.T.);
#11325=ORIENTED_EDGE('',*,*,#8282,.T.);
#11326=ORIENTED_EDGE('',*,*,#8265,.T.);
#11327=ORIENTED_EDGE('',*,*,#8291,.F.);
#11328=ORIENTED_EDGE('',*,*,#8268,.T.);
#11329=ORIENTED_EDGE('',*,*,#8277,.T.);
#11330=ORIENTED_EDGE('',*,*,#8289,.F.);
#11331=ORIENTED_EDGE('',*,*,#8278,.T.);
#11332=ORIENTED_EDGE('',*,*,#8243,.F.);
#11333=ORIENTED_EDGE('',*,*,#8274,.F.);
#11334=ORIENTED_EDGE('',*,*,#8234,.F.);
#11335=ORIENTED_EDGE('',*,*,#8287,.T.);
#11336=ORIENTED_EDGE('',*,*,#8292,.T.);
#11337=ORIENTED_EDGE('',*,*,#8271,.T.);
#11338=ORIENTED_EDGE('',*,*,#8293,.T.);
#11339=ORIENTED_EDGE('',*,*,#8262,.T.);
#11340=ORIENTED_EDGE('',*,*,#8237,.F.);
#11341=ORIENTED_EDGE('',*,*,#8279,.T.);
#11342=ORIENTED_EDGE('',*,*,#8292,.F.);
#11343=ORIENTED_EDGE('',*,*,#8286,.T.);
#11344=ORIENTED_EDGE('',*,*,#8294,.T.);
#11345=ORIENTED_EDGE('',*,*,#8270,.T.);
#11346=ORIENTED_EDGE('',*,*,#8295,.T.);
#11347=ORIENTED_EDGE('',*,*,#8263,.T.);
#11348=ORIENTED_EDGE('',*,*,#8293,.F.);
#11349=ORIENTED_EDGE('',*,*,#8280,.T.);
#11350=ORIENTED_EDGE('',*,*,#8294,.F.);
#11351=ORIENTED_EDGE('',*,*,#8285,.T.);
#11352=ORIENTED_EDGE('',*,*,#8290,.T.);
#11353=ORIENTED_EDGE('',*,*,#8269,.T.);
#11354=ORIENTED_EDGE('',*,*,#8291,.T.);
#11355=ORIENTED_EDGE('',*,*,#8264,.T.);
#11356=ORIENTED_EDGE('',*,*,#8295,.F.);
#11357=ORIENTED_EDGE('',*,*,#8296,.F.);
#11358=ORIENTED_EDGE('',*,*,#8297,.T.);
#11359=ORIENTED_EDGE('',*,*,#8258,.T.);
#11360=ORIENTED_EDGE('',*,*,#8272,.T.);
#11361=ORIENTED_EDGE('',*,*,#8259,.T.);
#11362=ORIENTED_EDGE('',*,*,#8297,.F.);
#11363=ORIENTED_EDGE('',*,*,#8296,.T.);
#11364=ORIENTED_EDGE('',*,*,#8288,.F.);
#11365=ORIENTED_EDGE('',*,*,#8298,.F.);
#11366=ORIENTED_EDGE('',*,*,#8299,.T.);
#11367=ORIENTED_EDGE('',*,*,#8300,.T.);
#11368=ORIENTED_EDGE('',*,*,#8301,.T.);
#11369=ORIENTED_EDGE('',*,*,#8302,.F.);
#11370=ORIENTED_EDGE('',*,*,#8303,.T.);
#11371=ORIENTED_EDGE('',*,*,#8298,.T.);
#11372=ORIENTED_EDGE('',*,*,#8304,.T.);
#11373=ORIENTED_EDGE('',*,*,#8305,.F.);
#11374=ORIENTED_EDGE('',*,*,#8306,.T.);
#11375=ORIENTED_EDGE('',*,*,#8302,.T.);
#11376=ORIENTED_EDGE('',*,*,#8307,.T.);
#11377=ORIENTED_EDGE('',*,*,#8308,.F.);
#11378=ORIENTED_EDGE('',*,*,#8309,.T.);
#11379=ORIENTED_EDGE('',*,*,#8305,.T.);
#11380=ORIENTED_EDGE('',*,*,#8310,.T.);
#11381=ORIENTED_EDGE('',*,*,#8311,.F.);
#11382=ORIENTED_EDGE('',*,*,#8312,.T.);
#11383=ORIENTED_EDGE('',*,*,#8308,.T.);
#11384=ORIENTED_EDGE('',*,*,#8313,.T.);
#11385=ORIENTED_EDGE('',*,*,#8314,.F.);
#11386=ORIENTED_EDGE('',*,*,#8315,.T.);
#11387=ORIENTED_EDGE('',*,*,#8311,.T.);
#11388=ORIENTED_EDGE('',*,*,#8316,.T.);
#11389=ORIENTED_EDGE('',*,*,#8317,.F.);
#11390=ORIENTED_EDGE('',*,*,#8318,.T.);
#11391=ORIENTED_EDGE('',*,*,#8319,.F.);
#11392=ORIENTED_EDGE('',*,*,#8320,.F.);
#11393=ORIENTED_EDGE('',*,*,#8321,.F.);
#11394=ORIENTED_EDGE('',*,*,#8322,.T.);
#11395=ORIENTED_EDGE('',*,*,#8317,.T.);
#11396=ORIENTED_EDGE('',*,*,#8323,.F.);
#11397=ORIENTED_EDGE('',*,*,#8324,.F.);
#11398=ORIENTED_EDGE('',*,*,#8325,.T.);
#11399=ORIENTED_EDGE('',*,*,#8321,.T.);
#11400=ORIENTED_EDGE('',*,*,#8326,.F.);
#11401=ORIENTED_EDGE('',*,*,#8327,.F.);
#11402=ORIENTED_EDGE('',*,*,#8328,.T.);
#11403=ORIENTED_EDGE('',*,*,#8324,.T.);
#11404=ORIENTED_EDGE('',*,*,#8329,.F.);
#11405=ORIENTED_EDGE('',*,*,#8330,.F.);
#11406=ORIENTED_EDGE('',*,*,#8331,.T.);
#11407=ORIENTED_EDGE('',*,*,#8327,.T.);
#11408=ORIENTED_EDGE('',*,*,#8332,.F.);
#11409=ORIENTED_EDGE('',*,*,#8333,.F.);
#11410=ORIENTED_EDGE('',*,*,#8334,.T.);
#11411=ORIENTED_EDGE('',*,*,#8330,.T.);
#11412=ORIENTED_EDGE('',*,*,#8335,.F.);
#11413=ORIENTED_EDGE('',*,*,#8319,.T.);
#11414=ORIENTED_EDGE('',*,*,#8336,.T.);
#11415=ORIENTED_EDGE('',*,*,#8337,.F.);
#11416=ORIENTED_EDGE('',*,*,#8338,.F.);
#11417=ORIENTED_EDGE('',*,*,#8339,.T.);
#11418=ORIENTED_EDGE('',*,*,#8339,.F.);
#11419=ORIENTED_EDGE('',*,*,#8340,.F.);
#11420=ORIENTED_EDGE('',*,*,#8316,.F.);
#11421=ORIENTED_EDGE('',*,*,#8313,.F.);
#11422=ORIENTED_EDGE('',*,*,#8310,.F.);
#11423=ORIENTED_EDGE('',*,*,#8307,.F.);
#11424=ORIENTED_EDGE('',*,*,#8304,.F.);
#11425=ORIENTED_EDGE('',*,*,#8301,.F.);
#11426=ORIENTED_EDGE('',*,*,#8341,.F.);
#11427=ORIENTED_EDGE('',*,*,#8342,.T.);
#11428=ORIENTED_EDGE('',*,*,#8335,.T.);
#11429=ORIENTED_EDGE('',*,*,#8332,.T.);
#11430=ORIENTED_EDGE('',*,*,#8329,.T.);
#11431=ORIENTED_EDGE('',*,*,#8326,.T.);
#11432=ORIENTED_EDGE('',*,*,#8323,.T.);
#11433=ORIENTED_EDGE('',*,*,#8320,.T.);
#11434=ORIENTED_EDGE('',*,*,#8343,.T.);
#11435=ORIENTED_EDGE('',*,*,#8344,.T.);
#11436=ORIENTED_EDGE('',*,*,#8345,.T.);
#11437=ORIENTED_EDGE('',*,*,#8346,.T.);
#11438=ORIENTED_EDGE('',*,*,#8341,.T.);
#11439=ORIENTED_EDGE('',*,*,#8333,.T.);
#11440=ORIENTED_EDGE('',*,*,#8342,.F.);
#11441=ORIENTED_EDGE('',*,*,#8346,.F.);
#11442=ORIENTED_EDGE('',*,*,#8347,.T.);
#11443=ORIENTED_EDGE('',*,*,#8336,.F.);
#11444=ORIENTED_EDGE('',*,*,#8318,.F.);
#11445=ORIENTED_EDGE('',*,*,#8322,.F.);
#11446=ORIENTED_EDGE('',*,*,#8325,.F.);
#11447=ORIENTED_EDGE('',*,*,#8328,.F.);
#11448=ORIENTED_EDGE('',*,*,#8331,.F.);
#11449=ORIENTED_EDGE('',*,*,#8334,.F.);
#11450=ORIENTED_EDGE('',*,*,#8347,.F.);
#11451=ORIENTED_EDGE('',*,*,#8345,.F.);
#11452=ORIENTED_EDGE('',*,*,#8299,.F.);
#11453=ORIENTED_EDGE('',*,*,#8303,.F.);
#11454=ORIENTED_EDGE('',*,*,#8306,.F.);
#11455=ORIENTED_EDGE('',*,*,#8309,.F.);
#11456=ORIENTED_EDGE('',*,*,#8312,.F.);
#11457=ORIENTED_EDGE('',*,*,#8315,.F.);
#11458=ORIENTED_EDGE('',*,*,#8348,.F.);
#11459=ORIENTED_EDGE('',*,*,#8349,.F.);
#11460=ORIENTED_EDGE('',*,*,#8350,.F.);
#11461=ORIENTED_EDGE('',*,*,#8351,.F.);
#11462=ORIENTED_EDGE('',*,*,#8352,.F.);
#11463=ORIENTED_EDGE('',*,*,#8353,.F.);
#11464=ORIENTED_EDGE('',*,*,#8354,.F.);
#11465=ORIENTED_EDGE('',*,*,#8355,.F.);
#11466=ORIENTED_EDGE('',*,*,#8356,.F.);
#11467=ORIENTED_EDGE('',*,*,#8357,.F.);
#11468=ORIENTED_EDGE('',*,*,#8358,.F.);
#11469=ORIENTED_EDGE('',*,*,#8359,.F.);
#11470=ORIENTED_EDGE('',*,*,#8360,.F.);
#11471=ORIENTED_EDGE('',*,*,#8361,.T.);
#11472=ORIENTED_EDGE('',*,*,#8362,.F.);
#11473=ORIENTED_EDGE('',*,*,#8363,.F.);
#11474=ORIENTED_EDGE('',*,*,#8352,.T.);
#11475=ORIENTED_EDGE('',*,*,#8364,.F.);
#11476=ORIENTED_EDGE('',*,*,#8365,.F.);
#11477=ORIENTED_EDGE('',*,*,#8366,.F.);
#11478=ORIENTED_EDGE('',*,*,#8350,.T.);
#11479=ORIENTED_EDGE('',*,*,#8367,.F.);
#11480=ORIENTED_EDGE('',*,*,#8368,.F.);
#11481=ORIENTED_EDGE('',*,*,#8369,.F.);
#11482=ORIENTED_EDGE('',*,*,#8360,.T.);
#11483=ORIENTED_EDGE('',*,*,#8370,.F.);
#11484=ORIENTED_EDGE('',*,*,#8371,.F.);
#11485=ORIENTED_EDGE('',*,*,#8372,.F.);
#11486=ORIENTED_EDGE('',*,*,#8358,.T.);
#11487=ORIENTED_EDGE('',*,*,#8373,.F.);
#11488=ORIENTED_EDGE('',*,*,#8374,.F.);
#11489=ORIENTED_EDGE('',*,*,#8375,.F.);
#11490=ORIENTED_EDGE('',*,*,#8356,.T.);
#11491=ORIENTED_EDGE('',*,*,#8376,.F.);
#11492=ORIENTED_EDGE('',*,*,#8377,.F.);
#11493=ORIENTED_EDGE('',*,*,#8378,.F.);
#11494=ORIENTED_EDGE('',*,*,#8354,.T.);
#11495=ORIENTED_EDGE('',*,*,#8379,.F.);
#11496=ORIENTED_EDGE('',*,*,#8380,.F.);
#11497=ORIENTED_EDGE('',*,*,#8361,.F.);
#11498=ORIENTED_EDGE('',*,*,#8353,.T.);
#11499=ORIENTED_EDGE('',*,*,#8381,.F.);
#11500=ORIENTED_EDGE('',*,*,#8382,.F.);
#11501=ORIENTED_EDGE('',*,*,#8383,.T.);
#11502=ORIENTED_EDGE('',*,*,#8379,.T.);
#11503=ORIENTED_EDGE('',*,*,#8384,.T.);
#11504=ORIENTED_EDGE('',*,*,#8385,.T.);
#11505=ORIENTED_EDGE('',*,*,#8355,.T.);
#11506=ORIENTED_EDGE('',*,*,#8386,.F.);
#11507=ORIENTED_EDGE('',*,*,#8387,.F.);
#11508=ORIENTED_EDGE('',*,*,#8381,.T.);
#11509=ORIENTED_EDGE('',*,*,#8375,.T.);
#11510=ORIENTED_EDGE('',*,*,#8388,.T.);
#11511=ORIENTED_EDGE('',*,*,#8389,.F.);
#11512=ORIENTED_EDGE('',*,*,#8376,.T.);
#11513=ORIENTED_EDGE('',*,*,#8390,.T.);
#11514=ORIENTED_EDGE('',*,*,#8391,.T.);
#11515=ORIENTED_EDGE('',*,*,#8351,.T.);
#11516=ORIENTED_EDGE('',*,*,#8383,.F.);
#11517=ORIENTED_EDGE('',*,*,#8392,.F.);
#11518=ORIENTED_EDGE('',*,*,#8393,.T.);
#11519=ORIENTED_EDGE('',*,*,#8364,.T.);
#11520=ORIENTED_EDGE('',*,*,#8394,.T.);
#11521=ORIENTED_EDGE('',*,*,#8395,.T.);
#11522=ORIENTED_EDGE('',*,*,#8357,.T.);
#11523=ORIENTED_EDGE('',*,*,#8396,.F.);
#11524=ORIENTED_EDGE('',*,*,#8397,.F.);
#11525=ORIENTED_EDGE('',*,*,#8386,.T.);
#11526=ORIENTED_EDGE('',*,*,#8372,.T.);
#11527=ORIENTED_EDGE('',*,*,#8398,.T.);
#11528=ORIENTED_EDGE('',*,*,#8399,.F.);
#11529=ORIENTED_EDGE('',*,*,#8373,.T.);
#11530=ORIENTED_EDGE('',*,*,#8389,.T.);
#11531=ORIENTED_EDGE('',*,*,#8400,.T.);
#11532=ORIENTED_EDGE('',*,*,#8377,.T.);
#11533=ORIENTED_EDGE('',*,*,#8391,.F.);
#11534=ORIENTED_EDGE('',*,*,#8401,.F.);
#11535=ORIENTED_EDGE('',*,*,#8374,.T.);
#11536=ORIENTED_EDGE('',*,*,#8400,.F.);
#11537=ORIENTED_EDGE('',*,*,#8388,.F.);
#11538=ORIENTED_EDGE('',*,*,#8371,.T.);
#11539=ORIENTED_EDGE('',*,*,#8402,.F.);
#11540=ORIENTED_EDGE('',*,*,#8398,.F.);
#11541=ORIENTED_EDGE('',*,*,#8368,.T.);
#11542=ORIENTED_EDGE('',*,*,#8403,.F.);
#11543=ORIENTED_EDGE('',*,*,#8404,.F.);
#11544=ORIENTED_EDGE('',*,*,#8365,.T.);
#11545=ORIENTED_EDGE('',*,*,#8395,.F.);
#11546=ORIENTED_EDGE('',*,*,#8405,.F.);
#11547=ORIENTED_EDGE('',*,*,#8362,.T.);
#11548=ORIENTED_EDGE('',*,*,#8380,.T.);
#11549=ORIENTED_EDGE('',*,*,#8385,.F.);
#11550=ORIENTED_EDGE('',*,*,#8406,.F.);
#11551=ORIENTED_EDGE('',*,*,#8359,.T.);
#11552=ORIENTED_EDGE('',*,*,#8407,.F.);
#11553=ORIENTED_EDGE('',*,*,#8408,.F.);
#11554=ORIENTED_EDGE('',*,*,#8396,.T.);
#11555=ORIENTED_EDGE('',*,*,#8369,.T.);
#11556=ORIENTED_EDGE('',*,*,#8404,.T.);
#11557=ORIENTED_EDGE('',*,*,#8409,.F.);
#11558=ORIENTED_EDGE('',*,*,#8370,.T.);
#11559=ORIENTED_EDGE('',*,*,#8399,.T.);
#11560=ORIENTED_EDGE('',*,*,#8402,.T.);
#11561=ORIENTED_EDGE('',*,*,#8367,.T.);
#11562=ORIENTED_EDGE('',*,*,#8409,.T.);
#11563=ORIENTED_EDGE('',*,*,#8403,.T.);
#11564=ORIENTED_EDGE('',*,*,#8349,.T.);
#11565=ORIENTED_EDGE('',*,*,#8393,.F.);
#11566=ORIENTED_EDGE('',*,*,#8410,.F.);
#11567=ORIENTED_EDGE('',*,*,#8407,.T.);
#11568=ORIENTED_EDGE('',*,*,#8378,.T.);
#11569=ORIENTED_EDGE('',*,*,#8401,.T.);
#11570=ORIENTED_EDGE('',*,*,#8390,.F.);
#11571=ORIENTED_EDGE('',*,*,#8363,.T.);
#11572=ORIENTED_EDGE('',*,*,#8406,.T.);
#11573=ORIENTED_EDGE('',*,*,#8384,.F.);
#11574=ORIENTED_EDGE('',*,*,#8366,.T.);
#11575=ORIENTED_EDGE('',*,*,#8405,.T.);
#11576=ORIENTED_EDGE('',*,*,#8394,.F.);
#11577=ORIENTED_EDGE('',*,*,#8411,.F.);
#11578=ORIENTED_EDGE('',*,*,#8343,.F.);
#11579=ORIENTED_EDGE('',*,*,#8300,.F.);
#11580=ORIENTED_EDGE('',*,*,#8344,.F.);
#11581=ORIENTED_EDGE('',*,*,#8412,.T.);
#11582=ORIENTED_EDGE('',*,*,#8411,.T.);
#11583=ORIENTED_EDGE('',*,*,#8412,.F.);
#11584=ORIENTED_EDGE('',*,*,#8314,.T.);
#11585=ORIENTED_EDGE('',*,*,#8340,.T.);
#11586=ORIENTED_EDGE('',*,*,#8413,.F.);
#11587=ORIENTED_EDGE('',*,*,#8348,.T.);
#11588=ORIENTED_EDGE('',*,*,#8414,.F.);
#11589=ORIENTED_EDGE('',*,*,#8415,.T.);
#11590=ORIENTED_EDGE('',*,*,#8337,.T.);
#11591=ORIENTED_EDGE('',*,*,#8413,.T.);
#11592=ORIENTED_EDGE('',*,*,#8338,.T.);
#11593=ORIENTED_EDGE('',*,*,#8415,.F.);
#11594=ORIENTED_EDGE('',*,*,#8414,.T.);
#11595=ORIENTED_EDGE('',*,*,#8397,.T.);
#11596=ORIENTED_EDGE('',*,*,#8408,.T.);
#11597=ORIENTED_EDGE('',*,*,#8410,.T.);
#11598=ORIENTED_EDGE('',*,*,#8392,.T.);
#11599=ORIENTED_EDGE('',*,*,#8382,.T.);
#11600=ORIENTED_EDGE('',*,*,#8387,.T.);
#11601=ORIENTED_EDGE('',*,*,#8416,.F.);
#11602=ORIENTED_EDGE('',*,*,#8417,.T.);
#11603=ORIENTED_EDGE('',*,*,#8418,.T.);
#11604=ORIENTED_EDGE('',*,*,#8419,.T.);
#11605=ORIENTED_EDGE('',*,*,#8420,.F.);
#11606=ORIENTED_EDGE('',*,*,#8421,.T.);
#11607=ORIENTED_EDGE('',*,*,#8416,.T.);
#11608=ORIENTED_EDGE('',*,*,#8422,.T.);
#11609=ORIENTED_EDGE('',*,*,#8423,.F.);
#11610=ORIENTED_EDGE('',*,*,#8424,.T.);
#11611=ORIENTED_EDGE('',*,*,#8420,.T.);
#11612=ORIENTED_EDGE('',*,*,#8425,.T.);
#11613=ORIENTED_EDGE('',*,*,#8426,.F.);
#11614=ORIENTED_EDGE('',*,*,#8427,.T.);
#11615=ORIENTED_EDGE('',*,*,#8423,.T.);
#11616=ORIENTED_EDGE('',*,*,#8428,.T.);
#11617=ORIENTED_EDGE('',*,*,#8429,.F.);
#11618=ORIENTED_EDGE('',*,*,#8430,.T.);
#11619=ORIENTED_EDGE('',*,*,#8426,.T.);
#11620=ORIENTED_EDGE('',*,*,#8431,.T.);
#11621=ORIENTED_EDGE('',*,*,#8432,.F.);
#11622=ORIENTED_EDGE('',*,*,#8433,.T.);
#11623=ORIENTED_EDGE('',*,*,#8434,.F.);
#11624=ORIENTED_EDGE('',*,*,#8435,.F.);
#11625=ORIENTED_EDGE('',*,*,#8436,.T.);
#11626=ORIENTED_EDGE('',*,*,#8432,.T.);
#11627=ORIENTED_EDGE('',*,*,#8437,.F.);
#11628=ORIENTED_EDGE('',*,*,#8438,.F.);
#11629=ORIENTED_EDGE('',*,*,#8439,.F.);
#11630=ORIENTED_EDGE('',*,*,#8440,.T.);
#11631=ORIENTED_EDGE('',*,*,#8435,.T.);
#11632=ORIENTED_EDGE('',*,*,#8441,.F.);
#11633=ORIENTED_EDGE('',*,*,#8442,.F.);
#11634=ORIENTED_EDGE('',*,*,#8443,.T.);
#11635=ORIENTED_EDGE('',*,*,#8439,.T.);
#11636=ORIENTED_EDGE('',*,*,#8444,.F.);
#11637=ORIENTED_EDGE('',*,*,#8445,.F.);
#11638=ORIENTED_EDGE('',*,*,#8446,.T.);
#11639=ORIENTED_EDGE('',*,*,#8442,.T.);
#11640=ORIENTED_EDGE('',*,*,#8447,.F.);
#11641=ORIENTED_EDGE('',*,*,#8437,.T.);
#11642=ORIENTED_EDGE('',*,*,#8434,.T.);
#11643=ORIENTED_EDGE('',*,*,#8448,.T.);
#11644=ORIENTED_EDGE('',*,*,#8449,.F.);
#11645=ORIENTED_EDGE('',*,*,#8450,.F.);
#11646=ORIENTED_EDGE('',*,*,#8451,.T.);
#11647=ORIENTED_EDGE('',*,*,#8451,.F.);
#11648=ORIENTED_EDGE('',*,*,#8452,.F.);
#11649=ORIENTED_EDGE('',*,*,#8431,.F.);
#11650=ORIENTED_EDGE('',*,*,#8428,.F.);
#11651=ORIENTED_EDGE('',*,*,#8425,.F.);
#11652=ORIENTED_EDGE('',*,*,#8422,.F.);
#11653=ORIENTED_EDGE('',*,*,#8419,.F.);
#11654=ORIENTED_EDGE('',*,*,#8453,.F.);
#11655=ORIENTED_EDGE('',*,*,#8454,.T.);
#11656=ORIENTED_EDGE('',*,*,#8447,.T.);
#11657=ORIENTED_EDGE('',*,*,#8444,.T.);
#11658=ORIENTED_EDGE('',*,*,#8441,.T.);
#11659=ORIENTED_EDGE('',*,*,#8438,.T.);
#11660=ORIENTED_EDGE('',*,*,#8455,.T.);
#11661=ORIENTED_EDGE('',*,*,#8456,.T.);
#11662=ORIENTED_EDGE('',*,*,#8457,.T.);
#11663=ORIENTED_EDGE('',*,*,#8458,.T.);
#11664=ORIENTED_EDGE('',*,*,#8453,.T.);
#11665=ORIENTED_EDGE('',*,*,#8445,.T.);
#11666=ORIENTED_EDGE('',*,*,#8454,.F.);
#11667=ORIENTED_EDGE('',*,*,#8458,.F.);
#11668=ORIENTED_EDGE('',*,*,#8459,.T.);
#11669=ORIENTED_EDGE('',*,*,#8448,.F.);
#11670=ORIENTED_EDGE('',*,*,#8433,.F.);
#11671=ORIENTED_EDGE('',*,*,#8436,.F.);
#11672=ORIENTED_EDGE('',*,*,#8440,.F.);
#11673=ORIENTED_EDGE('',*,*,#8443,.F.);
#11674=ORIENTED_EDGE('',*,*,#8446,.F.);
#11675=ORIENTED_EDGE('',*,*,#8459,.F.);
#11676=ORIENTED_EDGE('',*,*,#8457,.F.);
#11677=ORIENTED_EDGE('',*,*,#8417,.F.);
#11678=ORIENTED_EDGE('',*,*,#8421,.F.);
#11679=ORIENTED_EDGE('',*,*,#8424,.F.);
#11680=ORIENTED_EDGE('',*,*,#8427,.F.);
#11681=ORIENTED_EDGE('',*,*,#8430,.F.);
#11682=ORIENTED_EDGE('',*,*,#8460,.F.);
#11683=ORIENTED_EDGE('',*,*,#8461,.F.);
#11684=ORIENTED_EDGE('',*,*,#8462,.F.);
#11685=ORIENTED_EDGE('',*,*,#8463,.F.);
#11686=ORIENTED_EDGE('',*,*,#8464,.F.);
#11687=ORIENTED_EDGE('',*,*,#8465,.F.);
#11688=ORIENTED_EDGE('',*,*,#8466,.F.);
#11689=ORIENTED_EDGE('',*,*,#8467,.F.);
#11690=ORIENTED_EDGE('',*,*,#8468,.F.);
#11691=ORIENTED_EDGE('',*,*,#8469,.F.);
#11692=ORIENTED_EDGE('',*,*,#8470,.F.);
#11693=ORIENTED_EDGE('',*,*,#8471,.F.);
#11694=ORIENTED_EDGE('',*,*,#8472,.F.);
#11695=ORIENTED_EDGE('',*,*,#8473,.T.);
#11696=ORIENTED_EDGE('',*,*,#8474,.F.);
#11697=ORIENTED_EDGE('',*,*,#8475,.F.);
#11698=ORIENTED_EDGE('',*,*,#8464,.T.);
#11699=ORIENTED_EDGE('',*,*,#8476,.F.);
#11700=ORIENTED_EDGE('',*,*,#8477,.F.);
#11701=ORIENTED_EDGE('',*,*,#8478,.F.);
#11702=ORIENTED_EDGE('',*,*,#8462,.T.);
#11703=ORIENTED_EDGE('',*,*,#8479,.F.);
#11704=ORIENTED_EDGE('',*,*,#8480,.F.);
#11705=ORIENTED_EDGE('',*,*,#8481,.F.);
#11706=ORIENTED_EDGE('',*,*,#8472,.T.);
#11707=ORIENTED_EDGE('',*,*,#8482,.F.);
#11708=ORIENTED_EDGE('',*,*,#8483,.F.);
#11709=ORIENTED_EDGE('',*,*,#8484,.F.);
#11710=ORIENTED_EDGE('',*,*,#8470,.T.);
#11711=ORIENTED_EDGE('',*,*,#8485,.F.);
#11712=ORIENTED_EDGE('',*,*,#8486,.F.);
#11713=ORIENTED_EDGE('',*,*,#8487,.F.);
#11714=ORIENTED_EDGE('',*,*,#8468,.T.);
#11715=ORIENTED_EDGE('',*,*,#8488,.F.);
#11716=ORIENTED_EDGE('',*,*,#8489,.F.);
#11717=ORIENTED_EDGE('',*,*,#8490,.F.);
#11718=ORIENTED_EDGE('',*,*,#8466,.T.);
#11719=ORIENTED_EDGE('',*,*,#8491,.F.);
#11720=ORIENTED_EDGE('',*,*,#8492,.F.);
#11721=ORIENTED_EDGE('',*,*,#8473,.F.);
#11722=ORIENTED_EDGE('',*,*,#8465,.T.);
#11723=ORIENTED_EDGE('',*,*,#8493,.F.);
#11724=ORIENTED_EDGE('',*,*,#8494,.F.);
#11725=ORIENTED_EDGE('',*,*,#8495,.T.);
#11726=ORIENTED_EDGE('',*,*,#8491,.T.);
#11727=ORIENTED_EDGE('',*,*,#8496,.T.);
#11728=ORIENTED_EDGE('',*,*,#8497,.T.);
#11729=ORIENTED_EDGE('',*,*,#8467,.T.);
#11730=ORIENTED_EDGE('',*,*,#8498,.F.);
#11731=ORIENTED_EDGE('',*,*,#8499,.F.);
#11732=ORIENTED_EDGE('',*,*,#8493,.T.);
#11733=ORIENTED_EDGE('',*,*,#8487,.T.);
#11734=ORIENTED_EDGE('',*,*,#8500,.T.);
#11735=ORIENTED_EDGE('',*,*,#8501,.F.);
#11736=ORIENTED_EDGE('',*,*,#8488,.T.);
#11737=ORIENTED_EDGE('',*,*,#8502,.T.);
#11738=ORIENTED_EDGE('',*,*,#8503,.T.);
#11739=ORIENTED_EDGE('',*,*,#8463,.T.);
#11740=ORIENTED_EDGE('',*,*,#8495,.F.);
#11741=ORIENTED_EDGE('',*,*,#8504,.F.);
#11742=ORIENTED_EDGE('',*,*,#8505,.T.);
#11743=ORIENTED_EDGE('',*,*,#8476,.T.);
#11744=ORIENTED_EDGE('',*,*,#8506,.T.);
#11745=ORIENTED_EDGE('',*,*,#8507,.T.);
#11746=ORIENTED_EDGE('',*,*,#8469,.T.);
#11747=ORIENTED_EDGE('',*,*,#8508,.F.);
#11748=ORIENTED_EDGE('',*,*,#8509,.F.);
#11749=ORIENTED_EDGE('',*,*,#8498,.T.);
#11750=ORIENTED_EDGE('',*,*,#8484,.T.);
#11751=ORIENTED_EDGE('',*,*,#8510,.T.);
#11752=ORIENTED_EDGE('',*,*,#8511,.F.);
#11753=ORIENTED_EDGE('',*,*,#8485,.T.);
#11754=ORIENTED_EDGE('',*,*,#8501,.T.);
#11755=ORIENTED_EDGE('',*,*,#8512,.T.);
#11756=ORIENTED_EDGE('',*,*,#8489,.T.);
#11757=ORIENTED_EDGE('',*,*,#8503,.F.);
#11758=ORIENTED_EDGE('',*,*,#8513,.F.);
#11759=ORIENTED_EDGE('',*,*,#8486,.T.);
#11760=ORIENTED_EDGE('',*,*,#8512,.F.);
#11761=ORIENTED_EDGE('',*,*,#8500,.F.);
#11762=ORIENTED_EDGE('',*,*,#8483,.T.);
#11763=ORIENTED_EDGE('',*,*,#8514,.F.);
#11764=ORIENTED_EDGE('',*,*,#8510,.F.);
#11765=ORIENTED_EDGE('',*,*,#8480,.T.);
#11766=ORIENTED_EDGE('',*,*,#8515,.F.);
#11767=ORIENTED_EDGE('',*,*,#8516,.F.);
#11768=ORIENTED_EDGE('',*,*,#8477,.T.);
#11769=ORIENTED_EDGE('',*,*,#8507,.F.);
#11770=ORIENTED_EDGE('',*,*,#8517,.F.);
#11771=ORIENTED_EDGE('',*,*,#8474,.T.);
#11772=ORIENTED_EDGE('',*,*,#8492,.T.);
#11773=ORIENTED_EDGE('',*,*,#8497,.F.);
#11774=ORIENTED_EDGE('',*,*,#8518,.F.);
#11775=ORIENTED_EDGE('',*,*,#8471,.T.);
#11776=ORIENTED_EDGE('',*,*,#8519,.F.);
#11777=ORIENTED_EDGE('',*,*,#8520,.F.);
#11778=ORIENTED_EDGE('',*,*,#8508,.T.);
#11779=ORIENTED_EDGE('',*,*,#8481,.T.);
#11780=ORIENTED_EDGE('',*,*,#8516,.T.);
#11781=ORIENTED_EDGE('',*,*,#8521,.F.);
#11782=ORIENTED_EDGE('',*,*,#8482,.T.);
#11783=ORIENTED_EDGE('',*,*,#8511,.T.);
#11784=ORIENTED_EDGE('',*,*,#8514,.T.);
#11785=ORIENTED_EDGE('',*,*,#8479,.T.);
#11786=ORIENTED_EDGE('',*,*,#8521,.T.);
#11787=ORIENTED_EDGE('',*,*,#8515,.T.);
#11788=ORIENTED_EDGE('',*,*,#8461,.T.);
#11789=ORIENTED_EDGE('',*,*,#8505,.F.);
#11790=ORIENTED_EDGE('',*,*,#8522,.F.);
#11791=ORIENTED_EDGE('',*,*,#8519,.T.);
#11792=ORIENTED_EDGE('',*,*,#8490,.T.);
#11793=ORIENTED_EDGE('',*,*,#8513,.T.);
#11794=ORIENTED_EDGE('',*,*,#8502,.F.);
#11795=ORIENTED_EDGE('',*,*,#8475,.T.);
#11796=ORIENTED_EDGE('',*,*,#8518,.T.);
#11797=ORIENTED_EDGE('',*,*,#8496,.F.);
#11798=ORIENTED_EDGE('',*,*,#8478,.T.);
#11799=ORIENTED_EDGE('',*,*,#8517,.T.);
#11800=ORIENTED_EDGE('',*,*,#8506,.F.);
#11801=ORIENTED_EDGE('',*,*,#8523,.F.);
#11802=ORIENTED_EDGE('',*,*,#8455,.F.);
#11803=ORIENTED_EDGE('',*,*,#8418,.F.);
#11804=ORIENTED_EDGE('',*,*,#8456,.F.);
#11805=ORIENTED_EDGE('',*,*,#8524,.T.);
#11806=ORIENTED_EDGE('',*,*,#8523,.T.);
#11807=ORIENTED_EDGE('',*,*,#8524,.F.);
#11808=ORIENTED_EDGE('',*,*,#8429,.T.);
#11809=ORIENTED_EDGE('',*,*,#8452,.T.);
#11810=ORIENTED_EDGE('',*,*,#8525,.F.);
#11811=ORIENTED_EDGE('',*,*,#8460,.T.);
#11812=ORIENTED_EDGE('',*,*,#8526,.F.);
#11813=ORIENTED_EDGE('',*,*,#8527,.T.);
#11814=ORIENTED_EDGE('',*,*,#8449,.T.);
#11815=ORIENTED_EDGE('',*,*,#8525,.T.);
#11816=ORIENTED_EDGE('',*,*,#8450,.T.);
#11817=ORIENTED_EDGE('',*,*,#8527,.F.);
#11818=ORIENTED_EDGE('',*,*,#8526,.T.);
#11819=ORIENTED_EDGE('',*,*,#8509,.T.);
#11820=ORIENTED_EDGE('',*,*,#8520,.T.);
#11821=ORIENTED_EDGE('',*,*,#8522,.T.);
#11822=ORIENTED_EDGE('',*,*,#8504,.T.);
#11823=ORIENTED_EDGE('',*,*,#8494,.T.);
#11824=ORIENTED_EDGE('',*,*,#8499,.T.);
#11825=ORIENTED_EDGE('',*,*,#8528,.T.);
#11826=ORIENTED_EDGE('',*,*,#8529,.T.);
#11827=ORIENTED_EDGE('',*,*,#8530,.T.);
#11828=ORIENTED_EDGE('',*,*,#8531,.T.);
#11829=ORIENTED_EDGE('',*,*,#8532,.T.);
#11830=ORIENTED_EDGE('',*,*,#8533,.T.);
#11831=ORIENTED_EDGE('',*,*,#8531,.F.);
#11832=ORIENTED_EDGE('',*,*,#8534,.F.);
#11833=ORIENTED_EDGE('',*,*,#8535,.T.);
#11834=ORIENTED_EDGE('',*,*,#8536,.F.);
#11835=ORIENTED_EDGE('',*,*,#8537,.T.);
#11836=ORIENTED_EDGE('',*,*,#8530,.F.);
#11837=ORIENTED_EDGE('',*,*,#8538,.T.);
#11838=ORIENTED_EDGE('',*,*,#8539,.T.);
#11839=ORIENTED_EDGE('',*,*,#8540,.T.);
#11840=ORIENTED_EDGE('',*,*,#8534,.T.);
#11841=ORIENTED_EDGE('',*,*,#8529,.F.);
#11842=ORIENTED_EDGE('',*,*,#8541,.F.);
#11843=ORIENTED_EDGE('',*,*,#8542,.F.);
#11844=ORIENTED_EDGE('',*,*,#8543,.F.);
#11845=ORIENTED_EDGE('',*,*,#8544,.T.);
#11846=ORIENTED_EDGE('',*,*,#8545,.T.);
#11847=ORIENTED_EDGE('',*,*,#8546,.T.);
#11848=ORIENTED_EDGE('',*,*,#8547,.T.);
#11849=ORIENTED_EDGE('',*,*,#8548,.T.);
#11850=ORIENTED_EDGE('',*,*,#8549,.T.);
#11851=ORIENTED_EDGE('',*,*,#8550,.T.);
#11852=ORIENTED_EDGE('',*,*,#8545,.F.);
#11853=ORIENTED_EDGE('',*,*,#8551,.T.);
#11854=ORIENTED_EDGE('',*,*,#8552,.T.);
#11855=ORIENTED_EDGE('',*,*,#8553,.T.);
#11856=ORIENTED_EDGE('',*,*,#8547,.F.);
#11857=ORIENTED_EDGE('',*,*,#8548,.F.);
#11858=ORIENTED_EDGE('',*,*,#8544,.F.);
#11859=ORIENTED_EDGE('',*,*,#8553,.F.);
#11860=ORIENTED_EDGE('',*,*,#8554,.F.);
#11861=ORIENTED_EDGE('',*,*,#8555,.T.);
#11862=ORIENTED_EDGE('',*,*,#8556,.T.);
#11863=ORIENTED_EDGE('',*,*,#8557,.F.);
#11864=ORIENTED_EDGE('',*,*,#8558,.T.);
#11865=ORIENTED_EDGE('',*,*,#8559,.T.);
#11866=ORIENTED_EDGE('',*,*,#8560,.T.);
#11867=ORIENTED_EDGE('',*,*,#8558,.F.);
#11868=ORIENTED_EDGE('',*,*,#8561,.T.);
#11869=ORIENTED_EDGE('',*,*,#8562,.F.);
#11870=ORIENTED_EDGE('',*,*,#8563,.T.);
#11871=ORIENTED_EDGE('',*,*,#8555,.F.);
#11872=ORIENTED_EDGE('',*,*,#8564,.F.);
#11873=ORIENTED_EDGE('',*,*,#8565,.F.);
#11874=ORIENTED_EDGE('',*,*,#8566,.F.);
#11875=ORIENTED_EDGE('',*,*,#8556,.F.);
#11876=ORIENTED_EDGE('',*,*,#8563,.F.);
#11877=ORIENTED_EDGE('',*,*,#8561,.F.);
#11878=ORIENTED_EDGE('',*,*,#8567,.F.);
#11879=ORIENTED_EDGE('',*,*,#8568,.F.);
#11880=ORIENTED_EDGE('',*,*,#8569,.T.);
#11881=ORIENTED_EDGE('',*,*,#8559,.F.);
#11882=ORIENTED_EDGE('',*,*,#8560,.F.);
#11883=ORIENTED_EDGE('',*,*,#8569,.F.);
#11884=ORIENTED_EDGE('',*,*,#8570,.T.);
#11885=ORIENTED_EDGE('',*,*,#8571,.T.);
#11886=ORIENTED_EDGE('',*,*,#8572,.F.);
#11887=ORIENTED_EDGE('',*,*,#8565,.T.);
#11888=ORIENTED_EDGE('',*,*,#8573,.T.);
#11889=ORIENTED_EDGE('',*,*,#8574,.T.);
#11890=ORIENTED_EDGE('',*,*,#8562,.T.);
#11891=ORIENTED_EDGE('',*,*,#8574,.F.);
#11892=ORIENTED_EDGE('',*,*,#8575,.F.);
#11893=ORIENTED_EDGE('',*,*,#8576,.T.);
#11894=ORIENTED_EDGE('',*,*,#8573,.F.);
#11895=ORIENTED_EDGE('',*,*,#8576,.F.);
#11896=ORIENTED_EDGE('',*,*,#8577,.T.);
#11897=ORIENTED_EDGE('',*,*,#8567,.T.);
#11898=ORIENTED_EDGE('',*,*,#8568,.T.);
#11899=ORIENTED_EDGE('',*,*,#8577,.F.);
#11900=ORIENTED_EDGE('',*,*,#8578,.T.);
#11901=ORIENTED_EDGE('',*,*,#8579,.T.);
#11902=ORIENTED_EDGE('',*,*,#8580,.T.);
#11903=ORIENTED_EDGE('',*,*,#8581,.F.);
#11904=ORIENTED_EDGE('',*,*,#8582,.T.);
#11905=ORIENTED_EDGE('',*,*,#8583,.T.);
#11906=ORIENTED_EDGE('',*,*,#8582,.F.);
#11907=ORIENTED_EDGE('',*,*,#8580,.F.);
#11908=ORIENTED_EDGE('',*,*,#8579,.F.);
#11909=ORIENTED_EDGE('',*,*,#8578,.F.);
#11910=ORIENTED_EDGE('',*,*,#8575,.T.);
#11911=ORIENTED_EDGE('',*,*,#8584,.T.);
#11912=ORIENTED_EDGE('',*,*,#8585,.T.);
#11913=ORIENTED_EDGE('',*,*,#8584,.F.);
#11914=ORIENTED_EDGE('',*,*,#8585,.F.);
#11915=ORIENTED_EDGE('',*,*,#8586,.F.);
#11916=ORIENTED_EDGE('',*,*,#8587,.T.);
#11917=ORIENTED_EDGE('',*,*,#8588,.T.);
#11918=ORIENTED_EDGE('',*,*,#8589,.T.);
#11919=ORIENTED_EDGE('',*,*,#8590,.T.);
#11920=ORIENTED_EDGE('',*,*,#8591,.T.);
#11921=ORIENTED_EDGE('',*,*,#8592,.T.);
#11922=ORIENTED_EDGE('',*,*,#8542,.T.);
#11923=ORIENTED_EDGE('',*,*,#8593,.T.);
#11924=ORIENTED_EDGE('',*,*,#8594,.T.);
#11925=ORIENTED_EDGE('',*,*,#8592,.F.);
#11926=ORIENTED_EDGE('',*,*,#8595,.T.);
#11927=ORIENTED_EDGE('',*,*,#8588,.F.);
#11928=ORIENTED_EDGE('',*,*,#8596,.T.);
#11929=ORIENTED_EDGE('',*,*,#8590,.F.);
#11930=ORIENTED_EDGE('',*,*,#8597,.T.);
#11931=ORIENTED_EDGE('',*,*,#8593,.F.);
#11932=ORIENTED_EDGE('',*,*,#8596,.F.);
#11933=ORIENTED_EDGE('',*,*,#8541,.T.);
#11934=ORIENTED_EDGE('',*,*,#8598,.F.);
#11935=ORIENTED_EDGE('',*,*,#8599,.F.);
#11936=ORIENTED_EDGE('',*,*,#8600,.T.);
#11937=ORIENTED_EDGE('',*,*,#8591,.F.);
#11938=ORIENTED_EDGE('',*,*,#8597,.F.);
#11939=ORIENTED_EDGE('',*,*,#8589,.F.);
#11940=ORIENTED_EDGE('',*,*,#8595,.F.);
#11941=ORIENTED_EDGE('',*,*,#8601,.T.);
#11942=ORIENTED_EDGE('',*,*,#8602,.T.);
#11943=ORIENTED_EDGE('',*,*,#8603,.T.);
#11944=ORIENTED_EDGE('',*,*,#8604,.T.);
#11945=ORIENTED_EDGE('',*,*,#8605,.T.);
#11946=ORIENTED_EDGE('',*,*,#8606,.T.);
#11947=ORIENTED_EDGE('',*,*,#8601,.F.);
#11948=ORIENTED_EDGE('',*,*,#8607,.T.);
#11949=ORIENTED_EDGE('',*,*,#8608,.T.);
#11950=ORIENTED_EDGE('',*,*,#8609,.T.);
#11951=ORIENTED_EDGE('',*,*,#8610,.T.);
#11952=ORIENTED_EDGE('',*,*,#8611,.T.);
#11953=ORIENTED_EDGE('',*,*,#8606,.F.);
#11954=ORIENTED_EDGE('',*,*,#8612,.T.);
#11955=ORIENTED_EDGE('',*,*,#8613,.F.);
#11956=ORIENTED_EDGE('',*,*,#8614,.F.);
#11957=ORIENTED_EDGE('',*,*,#8615,.F.);
#11958=ORIENTED_EDGE('',*,*,#8607,.F.);
#11959=ORIENTED_EDGE('',*,*,#8605,.F.);
#11960=ORIENTED_EDGE('',*,*,#8616,.F.);
#11961=ORIENTED_EDGE('',*,*,#8617,.F.);
#11962=ORIENTED_EDGE('',*,*,#8612,.F.);
#11963=ORIENTED_EDGE('',*,*,#8618,.T.);
#11964=ORIENTED_EDGE('',*,*,#8619,.T.);
#11965=ORIENTED_EDGE('',*,*,#8620,.T.);
#11966=ORIENTED_EDGE('',*,*,#8539,.F.);
#11967=ORIENTED_EDGE('',*,*,#8603,.F.);
#11968=ORIENTED_EDGE('',*,*,#8621,.T.);
#11969=ORIENTED_EDGE('',*,*,#8619,.F.);
#11970=ORIENTED_EDGE('',*,*,#8622,.F.);
#11971=ORIENTED_EDGE('',*,*,#8623,.T.);
#11972=ORIENTED_EDGE('',*,*,#8624,.F.);
#11973=ORIENTED_EDGE('',*,*,#8625,.T.);
#11974=ORIENTED_EDGE('',*,*,#8550,.F.);
#11975=ORIENTED_EDGE('',*,*,#8626,.T.);
#11976=ORIENTED_EDGE('',*,*,#8622,.T.);
#11977=ORIENTED_EDGE('',*,*,#8618,.F.);
#11978=ORIENTED_EDGE('',*,*,#8627,.T.);
#11979=ORIENTED_EDGE('',*,*,#8628,.T.);
#11980=ORIENTED_EDGE('',*,*,#8594,.F.);
#11981=ORIENTED_EDGE('',*,*,#8629,.T.);
#11982=ORIENTED_EDGE('',*,*,#8627,.F.);
#11983=ORIENTED_EDGE('',*,*,#8538,.F.);
#11984=ORIENTED_EDGE('',*,*,#8543,.T.);
#11985=ORIENTED_EDGE('',*,*,#8630,.T.);
#11986=ORIENTED_EDGE('',*,*,#8631,.T.);
#11987=ORIENTED_EDGE('',*,*,#8632,.T.);
#11988=ORIENTED_EDGE('',*,*,#8633,.T.);
#11989=ORIENTED_EDGE('',*,*,#8528,.F.);
#11990=ORIENTED_EDGE('',*,*,#8634,.T.);
#11991=ORIENTED_EDGE('',*,*,#8635,.T.);
#11992=ORIENTED_EDGE('',*,*,#8633,.F.);
#11993=ORIENTED_EDGE('',*,*,#8598,.T.);
#11994=ORIENTED_EDGE('',*,*,#8631,.F.);
#11995=ORIENTED_EDGE('',*,*,#8636,.T.);
#11996=ORIENTED_EDGE('',*,*,#8637,.F.);
#11997=ORIENTED_EDGE('',*,*,#8638,.T.);
#11998=ORIENTED_EDGE('',*,*,#8639,.F.);
#11999=ORIENTED_EDGE('',*,*,#8640,.T.);
#12000=ORIENTED_EDGE('',*,*,#8641,.F.);
#12001=ORIENTED_EDGE('',*,*,#8630,.F.);
#12002=ORIENTED_EDGE('',*,*,#8635,.F.);
#12003=ORIENTED_EDGE('',*,*,#8642,.F.);
#12004=ORIENTED_EDGE('',*,*,#8643,.F.);
#12005=ORIENTED_EDGE('',*,*,#8644,.F.);
#12006=ORIENTED_EDGE('',*,*,#8645,.F.);
#12007=ORIENTED_EDGE('',*,*,#8636,.F.);
#12008=ORIENTED_EDGE('',*,*,#8533,.F.);
#12009=ORIENTED_EDGE('',*,*,#8646,.T.);
#12010=ORIENTED_EDGE('',*,*,#8647,.T.);
#12011=ORIENTED_EDGE('',*,*,#8642,.T.);
#12012=ORIENTED_EDGE('',*,*,#8634,.F.);
#12013=ORIENTED_EDGE('',*,*,#8637,.T.);
#12014=ORIENTED_EDGE('',*,*,#8645,.T.);
#12015=ORIENTED_EDGE('',*,*,#8648,.T.);
#12016=ORIENTED_EDGE('',*,*,#8613,.T.);
#12017=ORIENTED_EDGE('',*,*,#8617,.T.);
#12018=ORIENTED_EDGE('',*,*,#8649,.T.);
#12019=ORIENTED_EDGE('',*,*,#8648,.F.);
#12020=ORIENTED_EDGE('',*,*,#8644,.T.);
#12021=ORIENTED_EDGE('',*,*,#8650,.F.);
#12022=ORIENTED_EDGE('',*,*,#8651,.T.);
#12023=ORIENTED_EDGE('',*,*,#8652,.T.);
#12024=ORIENTED_EDGE('',*,*,#8614,.T.);
#12025=ORIENTED_EDGE('',*,*,#8653,.T.);
#12026=ORIENTED_EDGE('',*,*,#8654,.T.);
#12027=ORIENTED_EDGE('',*,*,#8655,.T.);
#12028=ORIENTED_EDGE('',*,*,#8656,.T.);
#12029=ORIENTED_EDGE('',*,*,#8657,.T.);
#12030=ORIENTED_EDGE('',*,*,#8658,.T.);
#12031=ORIENTED_EDGE('',*,*,#8659,.T.);
#12032=ORIENTED_EDGE('',*,*,#8660,.T.);
#12033=ORIENTED_EDGE('',*,*,#8661,.T.);
#12034=ORIENTED_EDGE('',*,*,#8662,.T.);
#12035=ORIENTED_EDGE('',*,*,#8658,.F.);
#12036=ORIENTED_EDGE('',*,*,#8663,.T.);
#12037=ORIENTED_EDGE('',*,*,#8656,.F.);
#12038=ORIENTED_EDGE('',*,*,#8664,.T.);
#12039=ORIENTED_EDGE('',*,*,#8665,.T.);
#12040=ORIENTED_EDGE('',*,*,#8660,.F.);
#12041=ORIENTED_EDGE('',*,*,#8666,.T.);
#12042=ORIENTED_EDGE('',*,*,#8667,.T.);
#12043=ORIENTED_EDGE('',*,*,#8668,.T.);
#12044=ORIENTED_EDGE('',*,*,#8654,.F.);
#12045=ORIENTED_EDGE('',*,*,#8667,.F.);
#12046=ORIENTED_EDGE('',*,*,#8669,.F.);
#12047=ORIENTED_EDGE('',*,*,#8670,.F.);
#12048=ORIENTED_EDGE('',*,*,#8659,.F.);
#12049=ORIENTED_EDGE('',*,*,#8662,.F.);
#12050=ORIENTED_EDGE('',*,*,#8671,.F.);
#12051=ORIENTED_EDGE('',*,*,#8672,.T.);
#12052=ORIENTED_EDGE('',*,*,#8669,.T.);
#12053=ORIENTED_EDGE('',*,*,#8666,.F.);
#12054=ORIENTED_EDGE('',*,*,#8651,.F.);
#12055=ORIENTED_EDGE('',*,*,#8673,.F.);
#12056=ORIENTED_EDGE('',*,*,#8609,.F.);
#12057=ORIENTED_EDGE('',*,*,#8674,.F.);
#12058=ORIENTED_EDGE('',*,*,#8675,.F.);
#12059=ORIENTED_EDGE('',*,*,#8676,.F.);
#12060=ORIENTED_EDGE('',*,*,#8677,.F.);
#12061=ORIENTED_EDGE('',*,*,#8678,.F.);
#12062=ORIENTED_EDGE('',*,*,#8657,.F.);
#12063=ORIENTED_EDGE('',*,*,#8665,.F.);
#12064=ORIENTED_EDGE('',*,*,#8653,.F.);
#12065=ORIENTED_EDGE('',*,*,#8663,.F.);
#12066=ORIENTED_EDGE('',*,*,#8675,.T.);
#12067=ORIENTED_EDGE('',*,*,#8679,.T.);
#12068=ORIENTED_EDGE('',*,*,#8680,.T.);
#12069=ORIENTED_EDGE('',*,*,#8679,.F.);
#12070=ORIENTED_EDGE('',*,*,#8681,.T.);
#12071=ORIENTED_EDGE('',*,*,#8680,.F.);
#12072=ORIENTED_EDGE('',*,*,#8681,.F.);
#12073=ORIENTED_EDGE('',*,*,#8678,.T.);
#12074=ORIENTED_EDGE('',*,*,#8682,.T.);
#12075=ORIENTED_EDGE('',*,*,#8683,.T.);
#12076=ORIENTED_EDGE('',*,*,#8682,.F.);
#12077=ORIENTED_EDGE('',*,*,#8683,.F.);
#12078=ORIENTED_EDGE('',*,*,#8684,.T.);
#12079=ORIENTED_EDGE('',*,*,#8685,.F.);
#12080=ORIENTED_EDGE('',*,*,#8684,.F.);
#12081=ORIENTED_EDGE('',*,*,#8676,.T.);
#12082=ORIENTED_EDGE('',*,*,#8686,.T.);
#12083=ORIENTED_EDGE('',*,*,#8687,.T.);
#12084=ORIENTED_EDGE('',*,*,#8686,.F.);
#12085=ORIENTED_EDGE('',*,*,#8687,.F.);
#12086=ORIENTED_EDGE('',*,*,#8688,.T.);
#12087=ORIENTED_EDGE('',*,*,#8689,.F.);
#12088=ORIENTED_EDGE('',*,*,#8688,.F.);
#12089=ORIENTED_EDGE('',*,*,#8647,.F.);
#12090=ORIENTED_EDGE('',*,*,#8690,.T.);
#12091=ORIENTED_EDGE('',*,*,#8650,.T.);
#12092=ORIENTED_EDGE('',*,*,#8643,.T.);
#12093=ORIENTED_EDGE('',*,*,#8615,.T.);
#12094=ORIENTED_EDGE('',*,*,#8652,.F.);
#12095=ORIENTED_EDGE('',*,*,#8674,.T.);
#12096=ORIENTED_EDGE('',*,*,#8608,.F.);
#12097=ORIENTED_EDGE('',*,*,#8610,.F.);
#12098=ORIENTED_EDGE('',*,*,#8691,.T.);
#12099=ORIENTED_EDGE('',*,*,#8536,.T.);
#12100=ORIENTED_EDGE('',*,*,#8692,.T.);
#12101=ORIENTED_EDGE('',*,*,#8602,.F.);
#12102=ORIENTED_EDGE('',*,*,#8611,.F.);
#12103=ORIENTED_EDGE('',*,*,#8692,.F.);
#12104=ORIENTED_EDGE('',*,*,#8535,.F.);
#12105=ORIENTED_EDGE('',*,*,#8540,.F.);
#12106=ORIENTED_EDGE('',*,*,#8620,.F.);
#12107=ORIENTED_EDGE('',*,*,#8621,.F.);
#12108=ORIENTED_EDGE('',*,*,#8693,.T.);
#12109=ORIENTED_EDGE('',*,*,#8694,.T.);
#12110=ORIENTED_EDGE('',*,*,#8677,.T.);
#12111=ORIENTED_EDGE('',*,*,#8694,.F.);
#12112=ORIENTED_EDGE('',*,*,#8693,.F.);
#12113=ORIENTED_EDGE('',*,*,#8695,.T.);
#12114=ORIENTED_EDGE('',*,*,#8696,.F.);
#12115=ORIENTED_EDGE('',*,*,#8695,.F.);
#12116=ORIENTED_EDGE('',*,*,#8697,.T.);
#12117=ORIENTED_EDGE('',*,*,#8698,.T.);
#12118=ORIENTED_EDGE('',*,*,#8685,.T.);
#12119=ORIENTED_EDGE('',*,*,#8698,.F.);
#12120=ORIENTED_EDGE('',*,*,#8699,.F.);
#12121=ORIENTED_EDGE('',*,*,#8700,.F.);
#12122=ORIENTED_EDGE('',*,*,#8701,.F.);
#12123=ORIENTED_EDGE('',*,*,#8702,.F.);
#12124=ORIENTED_EDGE('',*,*,#8703,.F.);
#12125=ORIENTED_EDGE('',*,*,#8704,.F.);
#12126=ORIENTED_EDGE('',*,*,#8697,.F.);
#12127=ORIENTED_EDGE('',*,*,#8703,.T.);
#12128=ORIENTED_EDGE('',*,*,#8705,.T.);
#12129=ORIENTED_EDGE('',*,*,#8689,.T.);
#12130=ORIENTED_EDGE('',*,*,#8705,.F.);
#12131=ORIENTED_EDGE('',*,*,#8706,.T.);
#12132=ORIENTED_EDGE('',*,*,#8707,.T.);
#12133=ORIENTED_EDGE('',*,*,#8701,.T.);
#12134=ORIENTED_EDGE('',*,*,#8708,.T.);
#12135=ORIENTED_EDGE('',*,*,#8699,.T.);
#12136=ORIENTED_EDGE('',*,*,#8709,.T.);
#12137=ORIENTED_EDGE('',*,*,#8710,.T.);
#12138=ORIENTED_EDGE('',*,*,#8711,.T.);
#12139=ORIENTED_EDGE('',*,*,#8624,.T.);
#12140=ORIENTED_EDGE('',*,*,#8709,.F.);
#12141=ORIENTED_EDGE('',*,*,#8702,.T.);
#12142=ORIENTED_EDGE('',*,*,#8707,.F.);
#12143=ORIENTED_EDGE('',*,*,#8639,.T.);
#12144=ORIENTED_EDGE('',*,*,#8708,.F.);
#12145=ORIENTED_EDGE('',*,*,#8700,.T.);
#12146=ORIENTED_EDGE('',*,*,#8711,.F.);
#12147=ORIENTED_EDGE('',*,*,#8549,.F.);
#12148=ORIENTED_EDGE('',*,*,#8557,.T.);
#12149=ORIENTED_EDGE('',*,*,#8566,.T.);
#12150=ORIENTED_EDGE('',*,*,#8572,.T.);
#12151=ORIENTED_EDGE('',*,*,#8712,.T.);
#12152=ORIENTED_EDGE('',*,*,#8570,.F.);
#12153=ORIENTED_EDGE('',*,*,#8564,.T.);
#12154=ORIENTED_EDGE('',*,*,#8554,.T.);
#12155=ORIENTED_EDGE('',*,*,#8552,.F.);
#12156=ORIENTED_EDGE('',*,*,#8713,.F.);
#12157=ORIENTED_EDGE('',*,*,#8640,.F.);
#12158=ORIENTED_EDGE('',*,*,#8710,.F.);
#12159=ORIENTED_EDGE('',*,*,#8623,.F.);
#12160=ORIENTED_EDGE('',*,*,#8626,.F.);
#12161=ORIENTED_EDGE('',*,*,#8696,.T.);
#12162=ORIENTED_EDGE('',*,*,#8714,.T.);
#12163=ORIENTED_EDGE('',*,*,#8715,.T.);
#12164=ORIENTED_EDGE('',*,*,#8714,.F.);
#12165=ORIENTED_EDGE('',*,*,#8716,.F.);
#12166=ORIENTED_EDGE('',*,*,#8717,.T.);
#12167=ORIENTED_EDGE('',*,*,#8715,.F.);
#12168=ORIENTED_EDGE('',*,*,#8717,.F.);
#12169=ORIENTED_EDGE('',*,*,#8718,.T.);
#12170=ORIENTED_EDGE('',*,*,#8719,.T.);
#12171=ORIENTED_EDGE('',*,*,#8704,.T.);
#12172=ORIENTED_EDGE('',*,*,#8719,.F.);
#12173=ORIENTED_EDGE('',*,*,#8718,.F.);
#12174=ORIENTED_EDGE('',*,*,#8720,.T.);
#12175=ORIENTED_EDGE('',*,*,#8721,.F.);
#12176=ORIENTED_EDGE('',*,*,#8720,.F.);
#12177=ORIENTED_EDGE('',*,*,#8721,.T.);
#12178=ORIENTED_EDGE('',*,*,#8722,.T.);
#12179=ORIENTED_EDGE('',*,*,#8716,.T.);
#12180=ORIENTED_EDGE('',*,*,#8722,.F.);
#12181=ORIENTED_EDGE('',*,*,#8655,.F.);
#12182=ORIENTED_EDGE('',*,*,#8668,.F.);
#12183=ORIENTED_EDGE('',*,*,#8670,.T.);
#12184=ORIENTED_EDGE('',*,*,#8672,.F.);
#12185=ORIENTED_EDGE('',*,*,#8723,.F.);
#12186=ORIENTED_EDGE('',*,*,#8664,.F.);
#12187=ORIENTED_EDGE('',*,*,#8661,.F.);
#12188=ORIENTED_EDGE('',*,*,#8723,.T.);
#12189=ORIENTED_EDGE('',*,*,#8671,.T.);
#12190=ORIENTED_EDGE('',*,*,#8586,.T.);
#12191=ORIENTED_EDGE('',*,*,#8724,.T.);
#12192=ORIENTED_EDGE('',*,*,#8581,.T.);
#12193=ORIENTED_EDGE('',*,*,#8724,.F.);
#12194=ORIENTED_EDGE('',*,*,#8583,.F.);
#12195=ORIENTED_EDGE('',*,*,#8571,.F.);
#12196=ORIENTED_EDGE('',*,*,#8712,.F.);
#12197=ORIENTED_EDGE('',*,*,#8546,.F.);
#12198=ORIENTED_EDGE('',*,*,#8628,.F.);
#12199=ORIENTED_EDGE('',*,*,#8629,.F.);
#12200=ORIENTED_EDGE('',*,*,#8587,.F.);
#12201=ORIENTED_EDGE('',*,*,#8600,.F.);
#12202=ORIENTED_EDGE('',*,*,#8725,.F.);
#12203=ORIENTED_EDGE('',*,*,#8551,.F.);
#12204=ORIENTED_EDGE('',*,*,#8725,.T.);
#12205=ORIENTED_EDGE('',*,*,#8599,.T.);
#12206=ORIENTED_EDGE('',*,*,#8632,.F.);
#12207=ORIENTED_EDGE('',*,*,#8641,.T.);
#12208=ORIENTED_EDGE('',*,*,#8713,.T.);
#12209=ORIENTED_EDGE('',*,*,#8604,.F.);
#12210=ORIENTED_EDGE('',*,*,#8625,.F.);
#12211=ORIENTED_EDGE('',*,*,#8706,.F.);
#12212=ORIENTED_EDGE('',*,*,#8638,.F.);
#12213=ORIENTED_EDGE('',*,*,#8649,.F.);
#12214=ORIENTED_EDGE('',*,*,#8616,.T.);
#12215=ORIENTED_EDGE('',*,*,#8532,.F.);
#12216=ORIENTED_EDGE('',*,*,#8537,.F.);
#12217=ORIENTED_EDGE('',*,*,#8726,.F.);
#12218=ORIENTED_EDGE('',*,*,#8646,.F.);
#12219=ORIENTED_EDGE('',*,*,#8690,.F.);
#12220=ORIENTED_EDGE('',*,*,#8726,.T.);
#12221=ORIENTED_EDGE('',*,*,#8691,.F.);
#12222=ORIENTED_EDGE('',*,*,#8673,.T.);
#12223=ORIENTED_EDGE('',*,*,#8727,.F.);
#12224=ORIENTED_EDGE('',*,*,#8728,.T.);
#12225=ORIENTED_EDGE('',*,*,#8729,.T.);
#12226=ORIENTED_EDGE('',*,*,#8730,.T.);
#12227=ORIENTED_EDGE('',*,*,#8731,.F.);
#12228=ORIENTED_EDGE('',*,*,#8732,.T.);
#12229=ORIENTED_EDGE('',*,*,#8727,.T.);
#12230=ORIENTED_EDGE('',*,*,#8733,.T.);
#12231=ORIENTED_EDGE('',*,*,#8734,.F.);
#12232=ORIENTED_EDGE('',*,*,#8735,.T.);
#12233=ORIENTED_EDGE('',*,*,#8731,.T.);
#12234=ORIENTED_EDGE('',*,*,#8736,.T.);
#12235=ORIENTED_EDGE('',*,*,#8737,.F.);
#12236=ORIENTED_EDGE('',*,*,#8738,.T.);
#12237=ORIENTED_EDGE('',*,*,#8734,.T.);
#12238=ORIENTED_EDGE('',*,*,#8739,.T.);
#12239=ORIENTED_EDGE('',*,*,#8740,.F.);
#12240=ORIENTED_EDGE('',*,*,#8741,.T.);
#12241=ORIENTED_EDGE('',*,*,#8737,.T.);
#12242=ORIENTED_EDGE('',*,*,#8742,.T.);
#12243=ORIENTED_EDGE('',*,*,#8743,.F.);
#12244=ORIENTED_EDGE('',*,*,#8744,.T.);
#12245=ORIENTED_EDGE('',*,*,#8740,.T.);
#12246=ORIENTED_EDGE('',*,*,#8745,.T.);
#12247=ORIENTED_EDGE('',*,*,#8746,.F.);
#12248=ORIENTED_EDGE('',*,*,#8747,.T.);
#12249=ORIENTED_EDGE('',*,*,#8743,.T.);
#12250=ORIENTED_EDGE('',*,*,#8748,.T.);
#12251=ORIENTED_EDGE('',*,*,#8749,.F.);
#12252=ORIENTED_EDGE('',*,*,#8750,.T.);
#12253=ORIENTED_EDGE('',*,*,#8746,.T.);
#12254=ORIENTED_EDGE('',*,*,#8751,.T.);
#12255=ORIENTED_EDGE('',*,*,#8752,.F.);
#12256=ORIENTED_EDGE('',*,*,#8753,.T.);
#12257=ORIENTED_EDGE('',*,*,#8749,.T.);
#12258=ORIENTED_EDGE('',*,*,#8754,.T.);
#12259=ORIENTED_EDGE('',*,*,#8755,.F.);
#12260=ORIENTED_EDGE('',*,*,#8756,.T.);
#12261=ORIENTED_EDGE('',*,*,#8752,.T.);
#12262=ORIENTED_EDGE('',*,*,#8757,.T.);
#12263=ORIENTED_EDGE('',*,*,#8758,.F.);
#12264=ORIENTED_EDGE('',*,*,#8759,.T.);
#12265=ORIENTED_EDGE('',*,*,#8755,.T.);
#12266=ORIENTED_EDGE('',*,*,#8760,.T.);
#12267=ORIENTED_EDGE('',*,*,#8761,.F.);
#12268=ORIENTED_EDGE('',*,*,#8762,.T.);
#12269=ORIENTED_EDGE('',*,*,#8758,.T.);
#12270=ORIENTED_EDGE('',*,*,#8763,.T.);
#12271=ORIENTED_EDGE('',*,*,#8764,.F.);
#12272=ORIENTED_EDGE('',*,*,#8765,.T.);
#12273=ORIENTED_EDGE('',*,*,#8761,.T.);
#12274=ORIENTED_EDGE('',*,*,#8766,.T.);
#12275=ORIENTED_EDGE('',*,*,#8767,.F.);
#12276=ORIENTED_EDGE('',*,*,#8768,.T.);
#12277=ORIENTED_EDGE('',*,*,#8764,.T.);
#12278=ORIENTED_EDGE('',*,*,#8769,.T.);
#12279=ORIENTED_EDGE('',*,*,#8770,.F.);
#12280=ORIENTED_EDGE('',*,*,#8771,.T.);
#12281=ORIENTED_EDGE('',*,*,#8767,.T.);
#12282=ORIENTED_EDGE('',*,*,#8772,.T.);
#12283=ORIENTED_EDGE('',*,*,#8773,.F.);
#12284=ORIENTED_EDGE('',*,*,#8774,.T.);
#12285=ORIENTED_EDGE('',*,*,#8770,.T.);
#12286=ORIENTED_EDGE('',*,*,#8775,.T.);
#12287=ORIENTED_EDGE('',*,*,#8776,.F.);
#12288=ORIENTED_EDGE('',*,*,#8777,.T.);
#12289=ORIENTED_EDGE('',*,*,#8773,.T.);
#12290=ORIENTED_EDGE('',*,*,#8778,.T.);
#12291=ORIENTED_EDGE('',*,*,#8779,.F.);
#12292=ORIENTED_EDGE('',*,*,#8780,.T.);
#12293=ORIENTED_EDGE('',*,*,#8776,.T.);
#12294=ORIENTED_EDGE('',*,*,#8781,.T.);
#12295=ORIENTED_EDGE('',*,*,#8782,.F.);
#12296=ORIENTED_EDGE('',*,*,#8783,.T.);
#12297=ORIENTED_EDGE('',*,*,#8779,.T.);
#12298=ORIENTED_EDGE('',*,*,#8784,.T.);
#12299=ORIENTED_EDGE('',*,*,#8785,.F.);
#12300=ORIENTED_EDGE('',*,*,#8786,.T.);
#12301=ORIENTED_EDGE('',*,*,#8782,.T.);
#12302=ORIENTED_EDGE('',*,*,#8787,.T.);
#12303=ORIENTED_EDGE('',*,*,#8788,.F.);
#12304=ORIENTED_EDGE('',*,*,#8789,.T.);
#12305=ORIENTED_EDGE('',*,*,#8785,.T.);
#12306=ORIENTED_EDGE('',*,*,#8790,.T.);
#12307=ORIENTED_EDGE('',*,*,#8791,.F.);
#12308=ORIENTED_EDGE('',*,*,#8792,.T.);
#12309=ORIENTED_EDGE('',*,*,#8788,.T.);
#12310=ORIENTED_EDGE('',*,*,#8793,.T.);
#12311=ORIENTED_EDGE('',*,*,#8794,.F.);
#12312=ORIENTED_EDGE('',*,*,#8795,.T.);
#12313=ORIENTED_EDGE('',*,*,#8791,.T.);
#12314=ORIENTED_EDGE('',*,*,#8796,.T.);
#12315=ORIENTED_EDGE('',*,*,#8797,.F.);
#12316=ORIENTED_EDGE('',*,*,#8798,.F.);
#12317=ORIENTED_EDGE('',*,*,#8799,.T.);
#12318=ORIENTED_EDGE('',*,*,#8794,.T.);
#12319=ORIENTED_EDGE('',*,*,#8800,.T.);
#12320=ORIENTED_EDGE('',*,*,#8801,.F.);
#12321=ORIENTED_EDGE('',*,*,#8802,.T.);
#12322=ORIENTED_EDGE('',*,*,#8803,.F.);
#12323=ORIENTED_EDGE('',*,*,#8804,.F.);
#12324=ORIENTED_EDGE('',*,*,#8805,.F.);
#12325=ORIENTED_EDGE('',*,*,#8806,.T.);
#12326=ORIENTED_EDGE('',*,*,#8801,.T.);
#12327=ORIENTED_EDGE('',*,*,#8807,.F.);
#12328=ORIENTED_EDGE('',*,*,#8808,.F.);
#12329=ORIENTED_EDGE('',*,*,#8809,.T.);
#12330=ORIENTED_EDGE('',*,*,#8805,.T.);
#12331=ORIENTED_EDGE('',*,*,#8810,.F.);
#12332=ORIENTED_EDGE('',*,*,#8811,.F.);
#12333=ORIENTED_EDGE('',*,*,#8812,.T.);
#12334=ORIENTED_EDGE('',*,*,#8808,.T.);
#12335=ORIENTED_EDGE('',*,*,#8813,.F.);
#12336=ORIENTED_EDGE('',*,*,#8814,.F.);
#12337=ORIENTED_EDGE('',*,*,#8815,.T.);
#12338=ORIENTED_EDGE('',*,*,#8811,.T.);
#12339=ORIENTED_EDGE('',*,*,#8816,.F.);
#12340=ORIENTED_EDGE('',*,*,#8817,.F.);
#12341=ORIENTED_EDGE('',*,*,#8818,.T.);
#12342=ORIENTED_EDGE('',*,*,#8814,.T.);
#12343=ORIENTED_EDGE('',*,*,#8819,.F.);
#12344=ORIENTED_EDGE('',*,*,#8820,.F.);
#12345=ORIENTED_EDGE('',*,*,#8821,.T.);
#12346=ORIENTED_EDGE('',*,*,#8817,.T.);
#12347=ORIENTED_EDGE('',*,*,#8822,.F.);
#12348=ORIENTED_EDGE('',*,*,#8823,.F.);
#12349=ORIENTED_EDGE('',*,*,#8824,.T.);
#12350=ORIENTED_EDGE('',*,*,#8820,.T.);
#12351=ORIENTED_EDGE('',*,*,#8825,.F.);
#12352=ORIENTED_EDGE('',*,*,#8826,.F.);
#12353=ORIENTED_EDGE('',*,*,#8827,.T.);
#12354=ORIENTED_EDGE('',*,*,#8823,.T.);
#12355=ORIENTED_EDGE('',*,*,#8828,.F.);
#12356=ORIENTED_EDGE('',*,*,#8829,.F.);
#12357=ORIENTED_EDGE('',*,*,#8830,.T.);
#12358=ORIENTED_EDGE('',*,*,#8826,.T.);
#12359=ORIENTED_EDGE('',*,*,#8831,.F.);
#12360=ORIENTED_EDGE('',*,*,#8832,.F.);
#12361=ORIENTED_EDGE('',*,*,#8833,.T.);
#12362=ORIENTED_EDGE('',*,*,#8829,.T.);
#12363=ORIENTED_EDGE('',*,*,#8834,.F.);
#12364=ORIENTED_EDGE('',*,*,#8835,.F.);
#12365=ORIENTED_EDGE('',*,*,#8836,.T.);
#12366=ORIENTED_EDGE('',*,*,#8832,.T.);
#12367=ORIENTED_EDGE('',*,*,#8837,.F.);
#12368=ORIENTED_EDGE('',*,*,#8838,.F.);
#12369=ORIENTED_EDGE('',*,*,#8839,.T.);
#12370=ORIENTED_EDGE('',*,*,#8835,.T.);
#12371=ORIENTED_EDGE('',*,*,#8840,.F.);
#12372=ORIENTED_EDGE('',*,*,#8841,.F.);
#12373=ORIENTED_EDGE('',*,*,#8842,.T.);
#12374=ORIENTED_EDGE('',*,*,#8838,.T.);
#12375=ORIENTED_EDGE('',*,*,#8843,.F.);
#12376=ORIENTED_EDGE('',*,*,#8844,.F.);
#12377=ORIENTED_EDGE('',*,*,#8845,.T.);
#12378=ORIENTED_EDGE('',*,*,#8841,.T.);
#12379=ORIENTED_EDGE('',*,*,#8846,.F.);
#12380=ORIENTED_EDGE('',*,*,#8847,.F.);
#12381=ORIENTED_EDGE('',*,*,#8848,.T.);
#12382=ORIENTED_EDGE('',*,*,#8844,.T.);
#12383=ORIENTED_EDGE('',*,*,#8849,.F.);
#12384=ORIENTED_EDGE('',*,*,#8850,.F.);
#12385=ORIENTED_EDGE('',*,*,#8851,.T.);
#12386=ORIENTED_EDGE('',*,*,#8847,.T.);
#12387=ORIENTED_EDGE('',*,*,#8852,.F.);
#12388=ORIENTED_EDGE('',*,*,#8853,.F.);
#12389=ORIENTED_EDGE('',*,*,#8854,.T.);
#12390=ORIENTED_EDGE('',*,*,#8850,.T.);
#12391=ORIENTED_EDGE('',*,*,#8855,.F.);
#12392=ORIENTED_EDGE('',*,*,#8856,.F.);
#12393=ORIENTED_EDGE('',*,*,#8857,.T.);
#12394=ORIENTED_EDGE('',*,*,#8853,.T.);
#12395=ORIENTED_EDGE('',*,*,#8858,.F.);
#12396=ORIENTED_EDGE('',*,*,#8859,.F.);
#12397=ORIENTED_EDGE('',*,*,#8860,.T.);
#12398=ORIENTED_EDGE('',*,*,#8856,.T.);
#12399=ORIENTED_EDGE('',*,*,#8861,.F.);
#12400=ORIENTED_EDGE('',*,*,#8862,.F.);
#12401=ORIENTED_EDGE('',*,*,#8863,.T.);
#12402=ORIENTED_EDGE('',*,*,#8859,.T.);
#12403=ORIENTED_EDGE('',*,*,#8864,.F.);
#12404=ORIENTED_EDGE('',*,*,#8865,.F.);
#12405=ORIENTED_EDGE('',*,*,#8866,.T.);
#12406=ORIENTED_EDGE('',*,*,#8862,.T.);
#12407=ORIENTED_EDGE('',*,*,#8867,.F.);
#12408=ORIENTED_EDGE('',*,*,#8868,.F.);
#12409=ORIENTED_EDGE('',*,*,#8869,.T.);
#12410=ORIENTED_EDGE('',*,*,#8865,.T.);
#12411=ORIENTED_EDGE('',*,*,#8870,.F.);
#12412=ORIENTED_EDGE('',*,*,#8871,.F.);
#12413=ORIENTED_EDGE('',*,*,#8872,.T.);
#12414=ORIENTED_EDGE('',*,*,#8873,.T.);
#12415=ORIENTED_EDGE('',*,*,#8874,.F.);
#12416=ORIENTED_EDGE('',*,*,#8875,.F.);
#12417=ORIENTED_EDGE('',*,*,#8876,.T.);
#12418=ORIENTED_EDGE('',*,*,#8877,.T.);
#12419=ORIENTED_EDGE('',*,*,#8872,.F.);
#12420=ORIENTED_EDGE('',*,*,#8878,.F.);
#12421=ORIENTED_EDGE('',*,*,#8879,.T.);
#12422=ORIENTED_EDGE('',*,*,#8880,.T.);
#12423=ORIENTED_EDGE('',*,*,#8876,.F.);
#12424=ORIENTED_EDGE('',*,*,#8881,.F.);
#12425=ORIENTED_EDGE('',*,*,#8874,.T.);
#12426=ORIENTED_EDGE('',*,*,#8882,.T.);
#12427=ORIENTED_EDGE('',*,*,#8879,.F.);
#12428=ORIENTED_EDGE('',*,*,#8882,.F.);
#12429=ORIENTED_EDGE('',*,*,#8873,.F.);
#12430=ORIENTED_EDGE('',*,*,#8877,.F.);
#12431=ORIENTED_EDGE('',*,*,#8880,.F.);
#12432=ORIENTED_EDGE('',*,*,#8883,.F.);
#12433=ORIENTED_EDGE('',*,*,#8884,.T.);
#12434=ORIENTED_EDGE('',*,*,#8885,.T.);
#12435=ORIENTED_EDGE('',*,*,#8884,.F.);
#12436=ORIENTED_EDGE('',*,*,#8885,.F.);
#12437=ORIENTED_EDGE('',*,*,#8886,.F.);
#12438=ORIENTED_EDGE('',*,*,#8887,.F.);
#12439=ORIENTED_EDGE('',*,*,#8800,.F.);
#12440=ORIENTED_EDGE('',*,*,#8796,.F.);
#12441=ORIENTED_EDGE('',*,*,#8793,.F.);
#12442=ORIENTED_EDGE('',*,*,#8790,.F.);
#12443=ORIENTED_EDGE('',*,*,#8787,.F.);
#12444=ORIENTED_EDGE('',*,*,#8784,.F.);
#12445=ORIENTED_EDGE('',*,*,#8781,.F.);
#12446=ORIENTED_EDGE('',*,*,#8778,.F.);
#12447=ORIENTED_EDGE('',*,*,#8775,.F.);
#12448=ORIENTED_EDGE('',*,*,#8772,.F.);
#12449=ORIENTED_EDGE('',*,*,#8769,.F.);
#12450=ORIENTED_EDGE('',*,*,#8766,.F.);
#12451=ORIENTED_EDGE('',*,*,#8763,.F.);
#12452=ORIENTED_EDGE('',*,*,#8760,.F.);
#12453=ORIENTED_EDGE('',*,*,#8757,.F.);
#12454=ORIENTED_EDGE('',*,*,#8754,.F.);
#12455=ORIENTED_EDGE('',*,*,#8751,.F.);
#12456=ORIENTED_EDGE('',*,*,#8748,.F.);
#12457=ORIENTED_EDGE('',*,*,#8745,.F.);
#12458=ORIENTED_EDGE('',*,*,#8742,.F.);
#12459=ORIENTED_EDGE('',*,*,#8739,.F.);
#12460=ORIENTED_EDGE('',*,*,#8736,.F.);
#12461=ORIENTED_EDGE('',*,*,#8733,.F.);
#12462=ORIENTED_EDGE('',*,*,#8730,.F.);
#12463=ORIENTED_EDGE('',*,*,#8888,.F.);
#12464=ORIENTED_EDGE('',*,*,#8889,.T.);
#12465=ORIENTED_EDGE('',*,*,#8870,.T.);
#12466=ORIENTED_EDGE('',*,*,#8867,.T.);
#12467=ORIENTED_EDGE('',*,*,#8864,.T.);
#12468=ORIENTED_EDGE('',*,*,#8861,.T.);
#12469=ORIENTED_EDGE('',*,*,#8858,.T.);
#12470=ORIENTED_EDGE('',*,*,#8855,.T.);
#12471=ORIENTED_EDGE('',*,*,#8852,.T.);
#12472=ORIENTED_EDGE('',*,*,#8849,.T.);
#12473=ORIENTED_EDGE('',*,*,#8846,.T.);
#12474=ORIENTED_EDGE('',*,*,#8843,.T.);
#12475=ORIENTED_EDGE('',*,*,#8840,.T.);
#12476=ORIENTED_EDGE('',*,*,#8837,.T.);
#12477=ORIENTED_EDGE('',*,*,#8834,.T.);
#12478=ORIENTED_EDGE('',*,*,#8831,.T.);
#12479=ORIENTED_EDGE('',*,*,#8828,.T.);
#12480=ORIENTED_EDGE('',*,*,#8825,.T.);
#12481=ORIENTED_EDGE('',*,*,#8822,.T.);
#12482=ORIENTED_EDGE('',*,*,#8819,.T.);
#12483=ORIENTED_EDGE('',*,*,#8816,.T.);
#12484=ORIENTED_EDGE('',*,*,#8813,.T.);
#12485=ORIENTED_EDGE('',*,*,#8810,.T.);
#12486=ORIENTED_EDGE('',*,*,#8807,.T.);
#12487=ORIENTED_EDGE('',*,*,#8804,.T.);
#12488=ORIENTED_EDGE('',*,*,#8890,.T.);
#12489=ORIENTED_EDGE('',*,*,#8891,.T.);
#12490=ORIENTED_EDGE('',*,*,#8892,.T.);
#12491=ORIENTED_EDGE('',*,*,#8893,.T.);
#12492=ORIENTED_EDGE('',*,*,#8888,.T.);
#12493=ORIENTED_EDGE('',*,*,#8868,.T.);
#12494=ORIENTED_EDGE('',*,*,#8889,.F.);
#12495=ORIENTED_EDGE('',*,*,#8893,.F.);
#12496=ORIENTED_EDGE('',*,*,#8894,.T.);
#12497=ORIENTED_EDGE('',*,*,#8895,.F.);
#12498=ORIENTED_EDGE('',*,*,#8802,.F.);
#12499=ORIENTED_EDGE('',*,*,#8806,.F.);
#12500=ORIENTED_EDGE('',*,*,#8809,.F.);
#12501=ORIENTED_EDGE('',*,*,#8812,.F.);
#12502=ORIENTED_EDGE('',*,*,#8815,.F.);
#12503=ORIENTED_EDGE('',*,*,#8818,.F.);
#12504=ORIENTED_EDGE('',*,*,#8821,.F.);
#12505=ORIENTED_EDGE('',*,*,#8824,.F.);
#12506=ORIENTED_EDGE('',*,*,#8827,.F.);
#12507=ORIENTED_EDGE('',*,*,#8830,.F.);
#12508=ORIENTED_EDGE('',*,*,#8833,.F.);
#12509=ORIENTED_EDGE('',*,*,#8836,.F.);
#12510=ORIENTED_EDGE('',*,*,#8839,.F.);
#12511=ORIENTED_EDGE('',*,*,#8842,.F.);
#12512=ORIENTED_EDGE('',*,*,#8845,.F.);
#12513=ORIENTED_EDGE('',*,*,#8848,.F.);
#12514=ORIENTED_EDGE('',*,*,#8851,.F.);
#12515=ORIENTED_EDGE('',*,*,#8854,.F.);
#12516=ORIENTED_EDGE('',*,*,#8857,.F.);
#12517=ORIENTED_EDGE('',*,*,#8860,.F.);
#12518=ORIENTED_EDGE('',*,*,#8863,.F.);
#12519=ORIENTED_EDGE('',*,*,#8866,.F.);
#12520=ORIENTED_EDGE('',*,*,#8869,.F.);
#12521=ORIENTED_EDGE('',*,*,#8894,.F.);
#12522=ORIENTED_EDGE('',*,*,#8892,.F.);
#12523=ORIENTED_EDGE('',*,*,#8728,.F.);
#12524=ORIENTED_EDGE('',*,*,#8732,.F.);
#12525=ORIENTED_EDGE('',*,*,#8735,.F.);
#12526=ORIENTED_EDGE('',*,*,#8738,.F.);
#12527=ORIENTED_EDGE('',*,*,#8741,.F.);
#12528=ORIENTED_EDGE('',*,*,#8744,.F.);
#12529=ORIENTED_EDGE('',*,*,#8747,.F.);
#12530=ORIENTED_EDGE('',*,*,#8750,.F.);
#12531=ORIENTED_EDGE('',*,*,#8753,.F.);
#12532=ORIENTED_EDGE('',*,*,#8756,.F.);
#12533=ORIENTED_EDGE('',*,*,#8759,.F.);
#12534=ORIENTED_EDGE('',*,*,#8762,.F.);
#12535=ORIENTED_EDGE('',*,*,#8765,.F.);
#12536=ORIENTED_EDGE('',*,*,#8768,.F.);
#12537=ORIENTED_EDGE('',*,*,#8771,.F.);
#12538=ORIENTED_EDGE('',*,*,#8774,.F.);
#12539=ORIENTED_EDGE('',*,*,#8777,.F.);
#12540=ORIENTED_EDGE('',*,*,#8780,.F.);
#12541=ORIENTED_EDGE('',*,*,#8783,.F.);
#12542=ORIENTED_EDGE('',*,*,#8786,.F.);
#12543=ORIENTED_EDGE('',*,*,#8789,.F.);
#12544=ORIENTED_EDGE('',*,*,#8792,.F.);
#12545=ORIENTED_EDGE('',*,*,#8795,.F.);
#12546=ORIENTED_EDGE('',*,*,#8799,.F.);
#12547=ORIENTED_EDGE('',*,*,#8896,.F.);
#12548=ORIENTED_EDGE('',*,*,#8897,.T.);
#12549=ORIENTED_EDGE('',*,*,#8898,.F.);
#12550=ORIENTED_EDGE('',*,*,#8899,.F.);
#12551=ORIENTED_EDGE('',*,*,#8900,.F.);
#12552=ORIENTED_EDGE('',*,*,#8901,.F.);
#12553=ORIENTED_EDGE('',*,*,#8902,.F.);
#12554=ORIENTED_EDGE('',*,*,#8897,.F.);
#12555=ORIENTED_EDGE('',*,*,#8903,.F.);
#12556=ORIENTED_EDGE('',*,*,#8904,.T.);
#12557=ORIENTED_EDGE('',*,*,#8905,.F.);
#12558=ORIENTED_EDGE('',*,*,#8906,.F.);
#12559=ORIENTED_EDGE('',*,*,#8907,.F.);
#12560=ORIENTED_EDGE('',*,*,#8908,.F.);
#12561=ORIENTED_EDGE('',*,*,#8909,.F.);
#12562=ORIENTED_EDGE('',*,*,#8904,.F.);
#12563=ORIENTED_EDGE('',*,*,#8910,.F.);
#12564=ORIENTED_EDGE('',*,*,#8911,.T.);
#12565=ORIENTED_EDGE('',*,*,#8912,.F.);
#12566=ORIENTED_EDGE('',*,*,#8913,.F.);
#12567=ORIENTED_EDGE('',*,*,#8914,.F.);
#12568=ORIENTED_EDGE('',*,*,#8915,.F.);
#12569=ORIENTED_EDGE('',*,*,#8916,.F.);
#12570=ORIENTED_EDGE('',*,*,#8911,.F.);
#12571=ORIENTED_EDGE('',*,*,#8917,.F.);
#12572=ORIENTED_EDGE('',*,*,#8918,.T.);
#12573=ORIENTED_EDGE('',*,*,#8919,.F.);
#12574=ORIENTED_EDGE('',*,*,#8920,.F.);
#12575=ORIENTED_EDGE('',*,*,#8921,.F.);
#12576=ORIENTED_EDGE('',*,*,#8922,.F.);
#12577=ORIENTED_EDGE('',*,*,#8923,.F.);
#12578=ORIENTED_EDGE('',*,*,#8918,.F.);
#12579=ORIENTED_EDGE('',*,*,#8924,.F.);
#12580=ORIENTED_EDGE('',*,*,#8925,.T.);
#12581=ORIENTED_EDGE('',*,*,#8926,.F.);
#12582=ORIENTED_EDGE('',*,*,#8927,.F.);
#12583=ORIENTED_EDGE('',*,*,#8928,.F.);
#12584=ORIENTED_EDGE('',*,*,#8929,.F.);
#12585=ORIENTED_EDGE('',*,*,#8930,.F.);
#12586=ORIENTED_EDGE('',*,*,#8925,.F.);
#12587=ORIENTED_EDGE('',*,*,#8931,.F.);
#12588=ORIENTED_EDGE('',*,*,#8932,.T.);
#12589=ORIENTED_EDGE('',*,*,#8933,.F.);
#12590=ORIENTED_EDGE('',*,*,#8934,.F.);
#12591=ORIENTED_EDGE('',*,*,#8935,.F.);
#12592=ORIENTED_EDGE('',*,*,#8936,.F.);
#12593=ORIENTED_EDGE('',*,*,#8937,.F.);
#12594=ORIENTED_EDGE('',*,*,#8932,.F.);
#12595=ORIENTED_EDGE('',*,*,#8938,.F.);
#12596=ORIENTED_EDGE('',*,*,#8939,.T.);
#12597=ORIENTED_EDGE('',*,*,#8940,.F.);
#12598=ORIENTED_EDGE('',*,*,#8941,.F.);
#12599=ORIENTED_EDGE('',*,*,#8942,.F.);
#12600=ORIENTED_EDGE('',*,*,#8943,.F.);
#12601=ORIENTED_EDGE('',*,*,#8944,.F.);
#12602=ORIENTED_EDGE('',*,*,#8939,.F.);
#12603=ORIENTED_EDGE('',*,*,#8945,.F.);
#12604=ORIENTED_EDGE('',*,*,#8946,.T.);
#12605=ORIENTED_EDGE('',*,*,#8947,.F.);
#12606=ORIENTED_EDGE('',*,*,#8948,.F.);
#12607=ORIENTED_EDGE('',*,*,#8949,.F.);
#12608=ORIENTED_EDGE('',*,*,#8950,.F.);
#12609=ORIENTED_EDGE('',*,*,#8951,.F.);
#12610=ORIENTED_EDGE('',*,*,#8946,.F.);
#12611=ORIENTED_EDGE('',*,*,#8952,.F.);
#12612=ORIENTED_EDGE('',*,*,#8953,.T.);
#12613=ORIENTED_EDGE('',*,*,#8954,.F.);
#12614=ORIENTED_EDGE('',*,*,#8955,.F.);
#12615=ORIENTED_EDGE('',*,*,#8956,.F.);
#12616=ORIENTED_EDGE('',*,*,#8957,.F.);
#12617=ORIENTED_EDGE('',*,*,#8958,.F.);
#12618=ORIENTED_EDGE('',*,*,#8953,.F.);
#12619=ORIENTED_EDGE('',*,*,#8959,.F.);
#12620=ORIENTED_EDGE('',*,*,#8960,.T.);
#12621=ORIENTED_EDGE('',*,*,#8961,.F.);
#12622=ORIENTED_EDGE('',*,*,#8962,.F.);
#12623=ORIENTED_EDGE('',*,*,#8963,.F.);
#12624=ORIENTED_EDGE('',*,*,#8964,.F.);
#12625=ORIENTED_EDGE('',*,*,#8965,.F.);
#12626=ORIENTED_EDGE('',*,*,#8960,.F.);
#12627=ORIENTED_EDGE('',*,*,#8966,.F.);
#12628=ORIENTED_EDGE('',*,*,#8967,.T.);
#12629=ORIENTED_EDGE('',*,*,#8968,.F.);
#12630=ORIENTED_EDGE('',*,*,#8969,.F.);
#12631=ORIENTED_EDGE('',*,*,#8970,.F.);
#12632=ORIENTED_EDGE('',*,*,#8971,.F.);
#12633=ORIENTED_EDGE('',*,*,#8972,.F.);
#12634=ORIENTED_EDGE('',*,*,#8967,.F.);
#12635=ORIENTED_EDGE('',*,*,#8973,.F.);
#12636=ORIENTED_EDGE('',*,*,#8974,.T.);
#12637=ORIENTED_EDGE('',*,*,#8975,.F.);
#12638=ORIENTED_EDGE('',*,*,#8976,.F.);
#12639=ORIENTED_EDGE('',*,*,#8977,.F.);
#12640=ORIENTED_EDGE('',*,*,#8978,.F.);
#12641=ORIENTED_EDGE('',*,*,#8979,.F.);
#12642=ORIENTED_EDGE('',*,*,#8974,.F.);
#12643=ORIENTED_EDGE('',*,*,#8980,.F.);
#12644=ORIENTED_EDGE('',*,*,#8981,.T.);
#12645=ORIENTED_EDGE('',*,*,#8982,.F.);
#12646=ORIENTED_EDGE('',*,*,#8983,.F.);
#12647=ORIENTED_EDGE('',*,*,#8984,.F.);
#12648=ORIENTED_EDGE('',*,*,#8985,.F.);
#12649=ORIENTED_EDGE('',*,*,#8986,.F.);
#12650=ORIENTED_EDGE('',*,*,#8981,.F.);
#12651=ORIENTED_EDGE('',*,*,#8987,.F.);
#12652=ORIENTED_EDGE('',*,*,#8988,.T.);
#12653=ORIENTED_EDGE('',*,*,#8989,.F.);
#12654=ORIENTED_EDGE('',*,*,#8990,.F.);
#12655=ORIENTED_EDGE('',*,*,#8991,.F.);
#12656=ORIENTED_EDGE('',*,*,#8992,.F.);
#12657=ORIENTED_EDGE('',*,*,#8993,.F.);
#12658=ORIENTED_EDGE('',*,*,#8988,.F.);
#12659=ORIENTED_EDGE('',*,*,#8994,.F.);
#12660=ORIENTED_EDGE('',*,*,#8995,.T.);
#12661=ORIENTED_EDGE('',*,*,#8996,.F.);
#12662=ORIENTED_EDGE('',*,*,#8997,.F.);
#12663=ORIENTED_EDGE('',*,*,#8998,.F.);
#12664=ORIENTED_EDGE('',*,*,#8999,.F.);
#12665=ORIENTED_EDGE('',*,*,#9000,.F.);
#12666=ORIENTED_EDGE('',*,*,#8995,.F.);
#12667=ORIENTED_EDGE('',*,*,#9001,.F.);
#12668=ORIENTED_EDGE('',*,*,#9002,.T.);
#12669=ORIENTED_EDGE('',*,*,#9003,.F.);
#12670=ORIENTED_EDGE('',*,*,#9004,.F.);
#12671=ORIENTED_EDGE('',*,*,#9005,.F.);
#12672=ORIENTED_EDGE('',*,*,#9006,.F.);
#12673=ORIENTED_EDGE('',*,*,#9007,.F.);
#12674=ORIENTED_EDGE('',*,*,#9002,.F.);
#12675=ORIENTED_EDGE('',*,*,#9008,.F.);
#12676=ORIENTED_EDGE('',*,*,#9009,.T.);
#12677=ORIENTED_EDGE('',*,*,#9010,.F.);
#12678=ORIENTED_EDGE('',*,*,#9011,.F.);
#12679=ORIENTED_EDGE('',*,*,#9012,.F.);
#12680=ORIENTED_EDGE('',*,*,#9013,.F.);
#12681=ORIENTED_EDGE('',*,*,#9014,.F.);
#12682=ORIENTED_EDGE('',*,*,#9009,.F.);
#12683=ORIENTED_EDGE('',*,*,#9015,.F.);
#12684=ORIENTED_EDGE('',*,*,#9016,.T.);
#12685=ORIENTED_EDGE('',*,*,#9017,.F.);
#12686=ORIENTED_EDGE('',*,*,#9018,.F.);
#12687=ORIENTED_EDGE('',*,*,#9019,.F.);
#12688=ORIENTED_EDGE('',*,*,#9020,.F.);
#12689=ORIENTED_EDGE('',*,*,#9021,.F.);
#12690=ORIENTED_EDGE('',*,*,#9016,.F.);
#12691=ORIENTED_EDGE('',*,*,#9022,.F.);
#12692=ORIENTED_EDGE('',*,*,#9023,.T.);
#12693=ORIENTED_EDGE('',*,*,#9024,.F.);
#12694=ORIENTED_EDGE('',*,*,#9025,.F.);
#12695=ORIENTED_EDGE('',*,*,#9026,.F.);
#12696=ORIENTED_EDGE('',*,*,#9027,.F.);
#12697=ORIENTED_EDGE('',*,*,#9028,.F.);
#12698=ORIENTED_EDGE('',*,*,#9023,.F.);
#12699=ORIENTED_EDGE('',*,*,#9029,.F.);
#12700=ORIENTED_EDGE('',*,*,#9030,.T.);
#12701=ORIENTED_EDGE('',*,*,#9031,.F.);
#12702=ORIENTED_EDGE('',*,*,#9032,.F.);
#12703=ORIENTED_EDGE('',*,*,#9033,.F.);
#12704=ORIENTED_EDGE('',*,*,#9034,.F.);
#12705=ORIENTED_EDGE('',*,*,#9035,.F.);
#12706=ORIENTED_EDGE('',*,*,#9030,.F.);
#12707=ORIENTED_EDGE('',*,*,#9036,.F.);
#12708=ORIENTED_EDGE('',*,*,#9037,.T.);
#12709=ORIENTED_EDGE('',*,*,#9038,.F.);
#12710=ORIENTED_EDGE('',*,*,#9039,.F.);
#12711=ORIENTED_EDGE('',*,*,#9040,.F.);
#12712=ORIENTED_EDGE('',*,*,#9041,.F.);
#12713=ORIENTED_EDGE('',*,*,#9042,.F.);
#12714=ORIENTED_EDGE('',*,*,#9037,.F.);
#12715=ORIENTED_EDGE('',*,*,#9043,.F.);
#12716=ORIENTED_EDGE('',*,*,#9044,.T.);
#12717=ORIENTED_EDGE('',*,*,#9045,.F.);
#12718=ORIENTED_EDGE('',*,*,#9046,.F.);
#12719=ORIENTED_EDGE('',*,*,#9047,.F.);
#12720=ORIENTED_EDGE('',*,*,#9048,.F.);
#12721=ORIENTED_EDGE('',*,*,#9049,.F.);
#12722=ORIENTED_EDGE('',*,*,#9044,.F.);
#12723=ORIENTED_EDGE('',*,*,#9050,.F.);
#12724=ORIENTED_EDGE('',*,*,#9051,.T.);
#12725=ORIENTED_EDGE('',*,*,#9052,.F.);
#12726=ORIENTED_EDGE('',*,*,#9053,.F.);
#12727=ORIENTED_EDGE('',*,*,#9054,.F.);
#12728=ORIENTED_EDGE('',*,*,#9055,.F.);
#12729=ORIENTED_EDGE('',*,*,#9056,.F.);
#12730=ORIENTED_EDGE('',*,*,#9051,.F.);
#12731=ORIENTED_EDGE('',*,*,#9057,.F.);
#12732=ORIENTED_EDGE('',*,*,#9058,.T.);
#12733=ORIENTED_EDGE('',*,*,#9059,.F.);
#12734=ORIENTED_EDGE('',*,*,#9060,.F.);
#12735=ORIENTED_EDGE('',*,*,#9061,.F.);
#12736=ORIENTED_EDGE('',*,*,#9062,.F.);
#12737=ORIENTED_EDGE('',*,*,#9063,.F.);
#12738=ORIENTED_EDGE('',*,*,#9058,.F.);
#12739=ORIENTED_EDGE('',*,*,#9064,.F.);
#12740=ORIENTED_EDGE('',*,*,#9065,.T.);
#12741=ORIENTED_EDGE('',*,*,#9066,.F.);
#12742=ORIENTED_EDGE('',*,*,#9067,.F.);
#12743=ORIENTED_EDGE('',*,*,#9068,.F.);
#12744=ORIENTED_EDGE('',*,*,#9069,.F.);
#12745=ORIENTED_EDGE('',*,*,#9070,.F.);
#12746=ORIENTED_EDGE('',*,*,#9065,.F.);
#12747=ORIENTED_EDGE('',*,*,#9071,.F.);
#12748=ORIENTED_EDGE('',*,*,#9072,.T.);
#12749=ORIENTED_EDGE('',*,*,#9073,.F.);
#12750=ORIENTED_EDGE('',*,*,#9074,.F.);
#12751=ORIENTED_EDGE('',*,*,#9075,.F.);
#12752=ORIENTED_EDGE('',*,*,#9076,.F.);
#12753=ORIENTED_EDGE('',*,*,#9077,.F.);
#12754=ORIENTED_EDGE('',*,*,#9072,.F.);
#12755=ORIENTED_EDGE('',*,*,#9078,.F.);
#12756=ORIENTED_EDGE('',*,*,#9079,.T.);
#12757=ORIENTED_EDGE('',*,*,#9080,.F.);
#12758=ORIENTED_EDGE('',*,*,#9081,.F.);
#12759=ORIENTED_EDGE('',*,*,#9082,.F.);
#12760=ORIENTED_EDGE('',*,*,#9083,.F.);
#12761=ORIENTED_EDGE('',*,*,#9084,.F.);
#12762=ORIENTED_EDGE('',*,*,#9079,.F.);
#12763=ORIENTED_EDGE('',*,*,#9085,.F.);
#12764=ORIENTED_EDGE('',*,*,#9086,.T.);
#12765=ORIENTED_EDGE('',*,*,#9087,.F.);
#12766=ORIENTED_EDGE('',*,*,#9088,.F.);
#12767=ORIENTED_EDGE('',*,*,#9089,.F.);
#12768=ORIENTED_EDGE('',*,*,#9090,.F.);
#12769=ORIENTED_EDGE('',*,*,#9091,.F.);
#12770=ORIENTED_EDGE('',*,*,#9086,.F.);
#12771=ORIENTED_EDGE('',*,*,#9092,.F.);
#12772=ORIENTED_EDGE('',*,*,#9093,.T.);
#12773=ORIENTED_EDGE('',*,*,#9094,.F.);
#12774=ORIENTED_EDGE('',*,*,#9095,.F.);
#12775=ORIENTED_EDGE('',*,*,#9096,.F.);
#12776=ORIENTED_EDGE('',*,*,#9097,.F.);
#12777=ORIENTED_EDGE('',*,*,#9098,.F.);
#12778=ORIENTED_EDGE('',*,*,#9093,.F.);
#12779=ORIENTED_EDGE('',*,*,#9099,.F.);
#12780=ORIENTED_EDGE('',*,*,#9100,.T.);
#12781=ORIENTED_EDGE('',*,*,#9101,.F.);
#12782=ORIENTED_EDGE('',*,*,#9102,.F.);
#12783=ORIENTED_EDGE('',*,*,#9103,.F.);
#12784=ORIENTED_EDGE('',*,*,#9104,.F.);
#12785=ORIENTED_EDGE('',*,*,#9105,.F.);
#12786=ORIENTED_EDGE('',*,*,#9100,.F.);
#12787=ORIENTED_EDGE('',*,*,#9046,.T.);
#12788=ORIENTED_EDGE('',*,*,#9106,.T.);
#12789=ORIENTED_EDGE('',*,*,#9055,.T.);
#12790=ORIENTED_EDGE('',*,*,#9107,.F.);
#12791=ORIENTED_EDGE('',*,*,#8997,.T.);
#12792=ORIENTED_EDGE('',*,*,#9108,.T.);
#12793=ORIENTED_EDGE('',*,*,#9006,.T.);
#12794=ORIENTED_EDGE('',*,*,#9109,.F.);
#12795=ORIENTED_EDGE('',*,*,#8992,.T.);
#12796=ORIENTED_EDGE('',*,*,#9110,.F.);
#12797=ORIENTED_EDGE('',*,*,#9004,.T.);
#12798=ORIENTED_EDGE('',*,*,#9111,.T.);
#12799=ORIENTED_EDGE('',*,*,#8990,.T.);
#12800=ORIENTED_EDGE('',*,*,#9112,.T.);
#12801=ORIENTED_EDGE('',*,*,#9013,.T.);
#12802=ORIENTED_EDGE('',*,*,#9113,.F.);
#12803=ORIENTED_EDGE('',*,*,#8985,.T.);
#12804=ORIENTED_EDGE('',*,*,#9114,.F.);
#12805=ORIENTED_EDGE('',*,*,#9011,.T.);
#12806=ORIENTED_EDGE('',*,*,#9115,.T.);
#12807=ORIENTED_EDGE('',*,*,#8983,.T.);
#12808=ORIENTED_EDGE('',*,*,#9116,.T.);
#12809=ORIENTED_EDGE('',*,*,#9020,.T.);
#12810=ORIENTED_EDGE('',*,*,#9117,.F.);
#12811=ORIENTED_EDGE('',*,*,#8978,.T.);
#12812=ORIENTED_EDGE('',*,*,#9118,.F.);
#12813=ORIENTED_EDGE('',*,*,#9018,.T.);
#12814=ORIENTED_EDGE('',*,*,#9119,.T.);
#12815=ORIENTED_EDGE('',*,*,#8976,.T.);
#12816=ORIENTED_EDGE('',*,*,#9120,.T.);
#12817=ORIENTED_EDGE('',*,*,#9027,.T.);
#12818=ORIENTED_EDGE('',*,*,#9121,.F.);
#12819=ORIENTED_EDGE('',*,*,#8971,.T.);
#12820=ORIENTED_EDGE('',*,*,#9122,.F.);
#12821=ORIENTED_EDGE('',*,*,#9025,.T.);
#12822=ORIENTED_EDGE('',*,*,#9123,.T.);
#12823=ORIENTED_EDGE('',*,*,#8969,.T.);
#12824=ORIENTED_EDGE('',*,*,#9124,.T.);
#12825=ORIENTED_EDGE('',*,*,#9034,.T.);
#12826=ORIENTED_EDGE('',*,*,#9125,.F.);
#12827=ORIENTED_EDGE('',*,*,#8964,.T.);
#12828=ORIENTED_EDGE('',*,*,#9126,.F.);
#12829=ORIENTED_EDGE('',*,*,#9032,.T.);
#12830=ORIENTED_EDGE('',*,*,#9127,.T.);
#12831=ORIENTED_EDGE('',*,*,#8962,.T.);
#12832=ORIENTED_EDGE('',*,*,#9128,.T.);
#12833=ORIENTED_EDGE('',*,*,#9041,.T.);
#12834=ORIENTED_EDGE('',*,*,#9129,.F.);
#12835=ORIENTED_EDGE('',*,*,#8957,.T.);
#12836=ORIENTED_EDGE('',*,*,#9130,.F.);
#12837=ORIENTED_EDGE('',*,*,#9039,.T.);
#12838=ORIENTED_EDGE('',*,*,#9131,.T.);
#12839=ORIENTED_EDGE('',*,*,#8955,.T.);
#12840=ORIENTED_EDGE('',*,*,#9132,.T.);
#12841=ORIENTED_EDGE('',*,*,#9048,.T.);
#12842=ORIENTED_EDGE('',*,*,#9133,.F.);
#12843=ORIENTED_EDGE('',*,*,#8950,.T.);
#12844=ORIENTED_EDGE('',*,*,#9134,.F.);
#12845=ORIENTED_EDGE('',*,*,#9102,.T.);
#12846=ORIENTED_EDGE('',*,*,#9135,.T.);
#12847=ORIENTED_EDGE('',*,*,#8948,.T.);
#12848=ORIENTED_EDGE('',*,*,#9136,.T.);
#12849=ORIENTED_EDGE('',*,*,#8999,.T.);
#12850=ORIENTED_EDGE('',*,*,#9137,.F.);
#12851=ORIENTED_EDGE('',*,*,#8943,.T.);
#12852=ORIENTED_EDGE('',*,*,#9138,.F.);
#12853=ORIENTED_EDGE('',*,*,#9053,.T.);
#12854=ORIENTED_EDGE('',*,*,#9139,.T.);
#12855=ORIENTED_EDGE('',*,*,#8941,.T.);
#12856=ORIENTED_EDGE('',*,*,#9140,.T.);
#12857=ORIENTED_EDGE('',*,*,#9062,.T.);
#12858=ORIENTED_EDGE('',*,*,#9141,.F.);
#12859=ORIENTED_EDGE('',*,*,#8936,.T.);
#12860=ORIENTED_EDGE('',*,*,#9142,.F.);
#12861=ORIENTED_EDGE('',*,*,#9060,.T.);
#12862=ORIENTED_EDGE('',*,*,#9143,.T.);
#12863=ORIENTED_EDGE('',*,*,#8934,.T.);
#12864=ORIENTED_EDGE('',*,*,#9144,.T.);
#12865=ORIENTED_EDGE('',*,*,#9069,.T.);
#12866=ORIENTED_EDGE('',*,*,#9145,.F.);
#12867=ORIENTED_EDGE('',*,*,#8929,.T.);
#12868=ORIENTED_EDGE('',*,*,#9146,.F.);
#12869=ORIENTED_EDGE('',*,*,#9067,.T.);
#12870=ORIENTED_EDGE('',*,*,#9147,.T.);
#12871=ORIENTED_EDGE('',*,*,#8927,.T.);
#12872=ORIENTED_EDGE('',*,*,#9148,.T.);
#12873=ORIENTED_EDGE('',*,*,#9076,.T.);
#12874=ORIENTED_EDGE('',*,*,#9149,.F.);
#12875=ORIENTED_EDGE('',*,*,#8922,.T.);
#12876=ORIENTED_EDGE('',*,*,#9150,.F.);
#12877=ORIENTED_EDGE('',*,*,#9074,.T.);
#12878=ORIENTED_EDGE('',*,*,#9151,.T.);
#12879=ORIENTED_EDGE('',*,*,#8920,.T.);
#12880=ORIENTED_EDGE('',*,*,#9152,.T.);
#12881=ORIENTED_EDGE('',*,*,#9083,.T.);
#12882=ORIENTED_EDGE('',*,*,#9153,.F.);
#12883=ORIENTED_EDGE('',*,*,#8915,.T.);
#12884=ORIENTED_EDGE('',*,*,#9154,.F.);
#12885=ORIENTED_EDGE('',*,*,#9081,.T.);
#12886=ORIENTED_EDGE('',*,*,#9155,.T.);
#12887=ORIENTED_EDGE('',*,*,#8913,.T.);
#12888=ORIENTED_EDGE('',*,*,#9156,.T.);
#12889=ORIENTED_EDGE('',*,*,#9090,.T.);
#12890=ORIENTED_EDGE('',*,*,#9157,.F.);
#12891=ORIENTED_EDGE('',*,*,#8908,.T.);
#12892=ORIENTED_EDGE('',*,*,#9158,.F.);
#12893=ORIENTED_EDGE('',*,*,#9088,.T.);
#12894=ORIENTED_EDGE('',*,*,#9159,.T.);
#12895=ORIENTED_EDGE('',*,*,#8906,.T.);
#12896=ORIENTED_EDGE('',*,*,#9160,.T.);
#12897=ORIENTED_EDGE('',*,*,#9097,.T.);
#12898=ORIENTED_EDGE('',*,*,#9161,.F.);
#12899=ORIENTED_EDGE('',*,*,#8901,.T.);
#12900=ORIENTED_EDGE('',*,*,#9162,.F.);
#12901=ORIENTED_EDGE('',*,*,#9095,.T.);
#12902=ORIENTED_EDGE('',*,*,#9163,.T.);
#12903=ORIENTED_EDGE('',*,*,#8899,.T.);
#12904=ORIENTED_EDGE('',*,*,#9164,.T.);
#12905=ORIENTED_EDGE('',*,*,#9104,.T.);
#12906=ORIENTED_EDGE('',*,*,#9165,.F.);
#12907=ORIENTED_EDGE('',*,*,#8898,.T.);
#12908=ORIENTED_EDGE('',*,*,#8902,.T.);
#12909=ORIENTED_EDGE('',*,*,#9163,.F.);
#12910=ORIENTED_EDGE('',*,*,#9094,.T.);
#12911=ORIENTED_EDGE('',*,*,#9098,.T.);
#12912=ORIENTED_EDGE('',*,*,#9160,.F.);
#12913=ORIENTED_EDGE('',*,*,#8905,.T.);
#12914=ORIENTED_EDGE('',*,*,#8909,.T.);
#12915=ORIENTED_EDGE('',*,*,#9159,.F.);
#12916=ORIENTED_EDGE('',*,*,#9087,.T.);
#12917=ORIENTED_EDGE('',*,*,#9091,.T.);
#12918=ORIENTED_EDGE('',*,*,#9156,.F.);
#12919=ORIENTED_EDGE('',*,*,#8912,.T.);
#12920=ORIENTED_EDGE('',*,*,#8916,.T.);
#12921=ORIENTED_EDGE('',*,*,#9155,.F.);
#12922=ORIENTED_EDGE('',*,*,#9080,.T.);
#12923=ORIENTED_EDGE('',*,*,#9084,.T.);
#12924=ORIENTED_EDGE('',*,*,#9152,.F.);
#12925=ORIENTED_EDGE('',*,*,#8919,.T.);
#12926=ORIENTED_EDGE('',*,*,#8923,.T.);
#12927=ORIENTED_EDGE('',*,*,#9151,.F.);
#12928=ORIENTED_EDGE('',*,*,#9073,.T.);
#12929=ORIENTED_EDGE('',*,*,#9077,.T.);
#12930=ORIENTED_EDGE('',*,*,#9148,.F.);
#12931=ORIENTED_EDGE('',*,*,#8926,.T.);
#12932=ORIENTED_EDGE('',*,*,#8930,.T.);
#12933=ORIENTED_EDGE('',*,*,#9147,.F.);
#12934=ORIENTED_EDGE('',*,*,#9066,.T.);
#12935=ORIENTED_EDGE('',*,*,#9070,.T.);
#12936=ORIENTED_EDGE('',*,*,#9144,.F.);
#12937=ORIENTED_EDGE('',*,*,#8933,.T.);
#12938=ORIENTED_EDGE('',*,*,#8937,.T.);
#12939=ORIENTED_EDGE('',*,*,#9143,.F.);
#12940=ORIENTED_EDGE('',*,*,#9059,.T.);
#12941=ORIENTED_EDGE('',*,*,#9063,.T.);
#12942=ORIENTED_EDGE('',*,*,#9140,.F.);
#12943=ORIENTED_EDGE('',*,*,#8940,.T.);
#12944=ORIENTED_EDGE('',*,*,#8944,.T.);
#12945=ORIENTED_EDGE('',*,*,#9139,.F.);
#12946=ORIENTED_EDGE('',*,*,#9052,.T.);
#12947=ORIENTED_EDGE('',*,*,#9166,.T.);
#12948=ORIENTED_EDGE('',*,*,#9167,.T.);
#12949=ORIENTED_EDGE('',*,*,#9166,.F.);
#12950=ORIENTED_EDGE('',*,*,#9056,.T.);
#12951=ORIENTED_EDGE('',*,*,#9106,.F.);
#12952=ORIENTED_EDGE('',*,*,#9045,.T.);
#12953=ORIENTED_EDGE('',*,*,#9049,.T.);
#12954=ORIENTED_EDGE('',*,*,#9132,.F.);
#12955=ORIENTED_EDGE('',*,*,#8954,.T.);
#12956=ORIENTED_EDGE('',*,*,#8958,.T.);
#12957=ORIENTED_EDGE('',*,*,#9131,.F.);
#12958=ORIENTED_EDGE('',*,*,#9038,.T.);
#12959=ORIENTED_EDGE('',*,*,#9042,.T.);
#12960=ORIENTED_EDGE('',*,*,#9128,.F.);
#12961=ORIENTED_EDGE('',*,*,#8961,.T.);
#12962=ORIENTED_EDGE('',*,*,#8965,.T.);
#12963=ORIENTED_EDGE('',*,*,#9127,.F.);
#12964=ORIENTED_EDGE('',*,*,#9031,.T.);
#12965=ORIENTED_EDGE('',*,*,#9035,.T.);
#12966=ORIENTED_EDGE('',*,*,#9124,.F.);
#12967=ORIENTED_EDGE('',*,*,#8968,.T.);
#12968=ORIENTED_EDGE('',*,*,#8972,.T.);
#12969=ORIENTED_EDGE('',*,*,#9123,.F.);
#12970=ORIENTED_EDGE('',*,*,#9024,.T.);
#12971=ORIENTED_EDGE('',*,*,#9028,.T.);
#12972=ORIENTED_EDGE('',*,*,#9120,.F.);
#12973=ORIENTED_EDGE('',*,*,#8975,.T.);
#12974=ORIENTED_EDGE('',*,*,#8979,.T.);
#12975=ORIENTED_EDGE('',*,*,#9119,.F.);
#12976=ORIENTED_EDGE('',*,*,#9017,.T.);
#12977=ORIENTED_EDGE('',*,*,#9021,.T.);
#12978=ORIENTED_EDGE('',*,*,#9116,.F.);
#12979=ORIENTED_EDGE('',*,*,#8982,.T.);
#12980=ORIENTED_EDGE('',*,*,#8986,.T.);
#12981=ORIENTED_EDGE('',*,*,#9115,.F.);
#12982=ORIENTED_EDGE('',*,*,#9010,.T.);
#12983=ORIENTED_EDGE('',*,*,#9014,.T.);
#12984=ORIENTED_EDGE('',*,*,#9112,.F.);
#12985=ORIENTED_EDGE('',*,*,#8989,.T.);
#12986=ORIENTED_EDGE('',*,*,#8993,.T.);
#12987=ORIENTED_EDGE('',*,*,#9111,.F.);
#12988=ORIENTED_EDGE('',*,*,#9003,.T.);
#12989=ORIENTED_EDGE('',*,*,#9007,.T.);
#12990=ORIENTED_EDGE('',*,*,#9108,.F.);
#12991=ORIENTED_EDGE('',*,*,#8996,.T.);
#12992=ORIENTED_EDGE('',*,*,#9000,.T.);
#12993=ORIENTED_EDGE('',*,*,#9136,.F.);
#12994=ORIENTED_EDGE('',*,*,#8947,.T.);
#12995=ORIENTED_EDGE('',*,*,#8951,.T.);
#12996=ORIENTED_EDGE('',*,*,#9135,.F.);
#12997=ORIENTED_EDGE('',*,*,#9101,.T.);
#12998=ORIENTED_EDGE('',*,*,#9105,.T.);
#12999=ORIENTED_EDGE('',*,*,#9164,.F.);
#13000=ORIENTED_EDGE('',*,*,#9168,.F.);
#13001=ORIENTED_EDGE('',*,*,#8883,.T.);
#13002=ORIENTED_EDGE('',*,*,#8890,.F.);
#13003=ORIENTED_EDGE('',*,*,#8729,.F.);
#13004=ORIENTED_EDGE('',*,*,#8891,.F.);
#13005=ORIENTED_EDGE('',*,*,#9169,.T.);
#13006=ORIENTED_EDGE('',*,*,#9168,.T.);
#13007=ORIENTED_EDGE('',*,*,#9169,.F.);
#13008=ORIENTED_EDGE('',*,*,#8797,.T.);
#13009=ORIENTED_EDGE('',*,*,#8887,.T.);
#13010=ORIENTED_EDGE('',*,*,#9170,.F.);
#13011=ORIENTED_EDGE('',*,*,#9167,.F.);
#13012=ORIENTED_EDGE('',*,*,#8798,.T.);
#13013=ORIENTED_EDGE('',*,*,#9170,.T.);
#13014=ORIENTED_EDGE('',*,*,#8886,.T.);
#13015=ORIENTED_EDGE('',*,*,#8803,.T.);
#13016=ORIENTED_EDGE('',*,*,#8895,.T.);
#13017=ORIENTED_EDGE('',*,*,#9171,.F.);
#13018=ORIENTED_EDGE('',*,*,#9172,.T.);
#13019=ORIENTED_EDGE('',*,*,#9050,.T.);
#13020=ORIENTED_EDGE('',*,*,#9138,.T.);
#13021=ORIENTED_EDGE('',*,*,#8942,.T.);
#13022=ORIENTED_EDGE('',*,*,#8938,.T.);
#13023=ORIENTED_EDGE('',*,*,#9141,.T.);
#13024=ORIENTED_EDGE('',*,*,#9061,.T.);
#13025=ORIENTED_EDGE('',*,*,#9057,.T.);
#13026=ORIENTED_EDGE('',*,*,#9142,.T.);
#13027=ORIENTED_EDGE('',*,*,#8935,.T.);
#13028=ORIENTED_EDGE('',*,*,#8931,.T.);
#13029=ORIENTED_EDGE('',*,*,#9145,.T.);
#13030=ORIENTED_EDGE('',*,*,#9068,.T.);
#13031=ORIENTED_EDGE('',*,*,#9064,.T.);
#13032=ORIENTED_EDGE('',*,*,#9146,.T.);
#13033=ORIENTED_EDGE('',*,*,#8928,.T.);
#13034=ORIENTED_EDGE('',*,*,#8924,.T.);
#13035=ORIENTED_EDGE('',*,*,#9149,.T.);
#13036=ORIENTED_EDGE('',*,*,#9075,.T.);
#13037=ORIENTED_EDGE('',*,*,#9071,.T.);
#13038=ORIENTED_EDGE('',*,*,#9150,.T.);
#13039=ORIENTED_EDGE('',*,*,#8921,.T.);
#13040=ORIENTED_EDGE('',*,*,#8917,.T.);
#13041=ORIENTED_EDGE('',*,*,#9153,.T.);
#13042=ORIENTED_EDGE('',*,*,#9082,.T.);
#13043=ORIENTED_EDGE('',*,*,#9078,.T.);
#13044=ORIENTED_EDGE('',*,*,#9154,.T.);
#13045=ORIENTED_EDGE('',*,*,#8914,.T.);
#13046=ORIENTED_EDGE('',*,*,#8910,.T.);
#13047=ORIENTED_EDGE('',*,*,#9157,.T.);
#13048=ORIENTED_EDGE('',*,*,#9089,.T.);
#13049=ORIENTED_EDGE('',*,*,#9085,.T.);
#13050=ORIENTED_EDGE('',*,*,#9158,.T.);
#13051=ORIENTED_EDGE('',*,*,#8907,.T.);
#13052=ORIENTED_EDGE('',*,*,#8903,.T.);
#13053=ORIENTED_EDGE('',*,*,#9161,.T.);
#13054=ORIENTED_EDGE('',*,*,#9096,.T.);
#13055=ORIENTED_EDGE('',*,*,#9092,.T.);
#13056=ORIENTED_EDGE('',*,*,#9162,.T.);
#13057=ORIENTED_EDGE('',*,*,#8900,.T.);
#13058=ORIENTED_EDGE('',*,*,#8896,.T.);
#13059=ORIENTED_EDGE('',*,*,#9165,.T.);
#13060=ORIENTED_EDGE('',*,*,#9103,.T.);
#13061=ORIENTED_EDGE('',*,*,#9099,.T.);
#13062=ORIENTED_EDGE('',*,*,#9134,.T.);
#13063=ORIENTED_EDGE('',*,*,#8949,.T.);
#13064=ORIENTED_EDGE('',*,*,#8945,.T.);
#13065=ORIENTED_EDGE('',*,*,#9137,.T.);
#13066=ORIENTED_EDGE('',*,*,#8998,.T.);
#13067=ORIENTED_EDGE('',*,*,#8994,.T.);
#13068=ORIENTED_EDGE('',*,*,#9109,.T.);
#13069=ORIENTED_EDGE('',*,*,#9005,.T.);
#13070=ORIENTED_EDGE('',*,*,#9001,.T.);
#13071=ORIENTED_EDGE('',*,*,#9110,.T.);
#13072=ORIENTED_EDGE('',*,*,#8991,.T.);
#13073=ORIENTED_EDGE('',*,*,#8987,.T.);
#13074=ORIENTED_EDGE('',*,*,#9113,.T.);
#13075=ORIENTED_EDGE('',*,*,#9012,.T.);
#13076=ORIENTED_EDGE('',*,*,#9008,.T.);
#13077=ORIENTED_EDGE('',*,*,#9114,.T.);
#13078=ORIENTED_EDGE('',*,*,#8984,.T.);
#13079=ORIENTED_EDGE('',*,*,#8980,.T.);
#13080=ORIENTED_EDGE('',*,*,#9117,.T.);
#13081=ORIENTED_EDGE('',*,*,#9019,.T.);
#13082=ORIENTED_EDGE('',*,*,#9015,.T.);
#13083=ORIENTED_EDGE('',*,*,#9118,.T.);
#13084=ORIENTED_EDGE('',*,*,#8977,.T.);
#13085=ORIENTED_EDGE('',*,*,#8973,.T.);
#13086=ORIENTED_EDGE('',*,*,#9121,.T.);
#13087=ORIENTED_EDGE('',*,*,#9026,.T.);
#13088=ORIENTED_EDGE('',*,*,#9022,.T.);
#13089=ORIENTED_EDGE('',*,*,#9122,.T.);
#13090=ORIENTED_EDGE('',*,*,#8970,.T.);
#13091=ORIENTED_EDGE('',*,*,#8966,.T.);
#13092=ORIENTED_EDGE('',*,*,#9125,.T.);
#13093=ORIENTED_EDGE('',*,*,#9033,.T.);
#13094=ORIENTED_EDGE('',*,*,#9029,.T.);
#13095=ORIENTED_EDGE('',*,*,#9126,.T.);
#13096=ORIENTED_EDGE('',*,*,#8963,.T.);
#13097=ORIENTED_EDGE('',*,*,#8959,.T.);
#13098=ORIENTED_EDGE('',*,*,#9129,.T.);
#13099=ORIENTED_EDGE('',*,*,#9040,.T.);
#13100=ORIENTED_EDGE('',*,*,#9036,.T.);
#13101=ORIENTED_EDGE('',*,*,#9130,.T.);
#13102=ORIENTED_EDGE('',*,*,#8956,.T.);
#13103=ORIENTED_EDGE('',*,*,#8952,.T.);
#13104=ORIENTED_EDGE('',*,*,#9133,.T.);
#13105=ORIENTED_EDGE('',*,*,#9047,.T.);
#13106=ORIENTED_EDGE('',*,*,#9043,.T.);
#13107=ORIENTED_EDGE('',*,*,#9107,.T.);
#13108=ORIENTED_EDGE('',*,*,#9054,.T.);
#13109=ORIENTED_EDGE('',*,*,#9172,.F.);
#13110=ORIENTED_EDGE('',*,*,#9171,.T.);
#13111=ORIENTED_EDGE('',*,*,#8871,.T.);
#13112=ORIENTED_EDGE('',*,*,#8881,.T.);
#13113=ORIENTED_EDGE('',*,*,#8878,.T.);
#13114=ORIENTED_EDGE('',*,*,#8875,.T.);
#13115=ORIENTED_EDGE('',*,*,#9173,.T.);
#13116=ORIENTED_EDGE('',*,*,#9173,.F.);
#13117=ORIENTED_EDGE('',*,*,#9174,.T.);
#13118=ORIENTED_EDGE('',*,*,#9175,.T.);
#13119=ORIENTED_EDGE('',*,*,#9176,.F.);
#13120=ORIENTED_EDGE('',*,*,#9175,.F.);
#13121=ORIENTED_EDGE('',*,*,#9176,.T.);
#13122=ORIENTED_EDGE('',*,*,#9174,.F.);
#13123=ORIENTED_EDGE('',*,*,#9177,.F.);
#13124=ORIENTED_EDGE('',*,*,#9178,.T.);
#13125=ORIENTED_EDGE('',*,*,#9179,.T.);
#13126=ORIENTED_EDGE('',*,*,#9180,.T.);
#13127=ORIENTED_EDGE('',*,*,#9181,.F.);
#13128=ORIENTED_EDGE('',*,*,#9182,.T.);
#13129=ORIENTED_EDGE('',*,*,#9177,.T.);
#13130=ORIENTED_EDGE('',*,*,#9183,.T.);
#13131=ORIENTED_EDGE('',*,*,#9184,.F.);
#13132=ORIENTED_EDGE('',*,*,#9185,.T.);
#13133=ORIENTED_EDGE('',*,*,#9181,.T.);
#13134=ORIENTED_EDGE('',*,*,#9186,.T.);
#13135=ORIENTED_EDGE('',*,*,#9187,.F.);
#13136=ORIENTED_EDGE('',*,*,#9188,.T.);
#13137=ORIENTED_EDGE('',*,*,#9184,.T.);
#13138=ORIENTED_EDGE('',*,*,#9189,.T.);
#13139=ORIENTED_EDGE('',*,*,#9190,.F.);
#13140=ORIENTED_EDGE('',*,*,#9191,.T.);
#13141=ORIENTED_EDGE('',*,*,#9187,.T.);
#13142=ORIENTED_EDGE('',*,*,#9192,.T.);
#13143=ORIENTED_EDGE('',*,*,#9193,.F.);
#13144=ORIENTED_EDGE('',*,*,#9194,.T.);
#13145=ORIENTED_EDGE('',*,*,#9190,.T.);
#13146=ORIENTED_EDGE('',*,*,#9195,.T.);
#13147=ORIENTED_EDGE('',*,*,#9196,.F.);
#13148=ORIENTED_EDGE('',*,*,#9197,.T.);
#13149=ORIENTED_EDGE('',*,*,#9193,.T.);
#13150=ORIENTED_EDGE('',*,*,#9198,.T.);
#13151=ORIENTED_EDGE('',*,*,#9199,.F.);
#13152=ORIENTED_EDGE('',*,*,#9200,.T.);
#13153=ORIENTED_EDGE('',*,*,#9196,.T.);
#13154=ORIENTED_EDGE('',*,*,#9201,.T.);
#13155=ORIENTED_EDGE('',*,*,#9202,.F.);
#13156=ORIENTED_EDGE('',*,*,#9203,.T.);
#13157=ORIENTED_EDGE('',*,*,#9199,.T.);
#13158=ORIENTED_EDGE('',*,*,#9204,.T.);
#13159=ORIENTED_EDGE('',*,*,#9205,.F.);
#13160=ORIENTED_EDGE('',*,*,#9206,.T.);
#13161=ORIENTED_EDGE('',*,*,#9202,.T.);
#13162=ORIENTED_EDGE('',*,*,#9207,.T.);
#13163=ORIENTED_EDGE('',*,*,#9208,.F.);
#13164=ORIENTED_EDGE('',*,*,#9209,.T.);
#13165=ORIENTED_EDGE('',*,*,#9205,.T.);
#13166=ORIENTED_EDGE('',*,*,#9210,.T.);
#13167=ORIENTED_EDGE('',*,*,#9211,.F.);
#13168=ORIENTED_EDGE('',*,*,#9212,.T.);
#13169=ORIENTED_EDGE('',*,*,#9208,.T.);
#13170=ORIENTED_EDGE('',*,*,#9213,.T.);
#13171=ORIENTED_EDGE('',*,*,#9214,.F.);
#13172=ORIENTED_EDGE('',*,*,#9215,.T.);
#13173=ORIENTED_EDGE('',*,*,#9211,.T.);
#13174=ORIENTED_EDGE('',*,*,#9216,.T.);
#13175=ORIENTED_EDGE('',*,*,#9217,.F.);
#13176=ORIENTED_EDGE('',*,*,#9218,.T.);
#13177=ORIENTED_EDGE('',*,*,#9214,.T.);
#13178=ORIENTED_EDGE('',*,*,#9219,.T.);
#13179=ORIENTED_EDGE('',*,*,#9220,.F.);
#13180=ORIENTED_EDGE('',*,*,#9221,.T.);
#13181=ORIENTED_EDGE('',*,*,#9217,.T.);
#13182=ORIENTED_EDGE('',*,*,#9222,.T.);
#13183=ORIENTED_EDGE('',*,*,#9223,.F.);
#13184=ORIENTED_EDGE('',*,*,#9224,.T.);
#13185=ORIENTED_EDGE('',*,*,#9220,.T.);
#13186=ORIENTED_EDGE('',*,*,#9225,.T.);
#13187=ORIENTED_EDGE('',*,*,#9226,.F.);
#13188=ORIENTED_EDGE('',*,*,#9227,.T.);
#13189=ORIENTED_EDGE('',*,*,#9223,.T.);
#13190=ORIENTED_EDGE('',*,*,#9228,.T.);
#13191=ORIENTED_EDGE('',*,*,#9229,.F.);
#13192=ORIENTED_EDGE('',*,*,#9230,.T.);
#13193=ORIENTED_EDGE('',*,*,#9226,.T.);
#13194=ORIENTED_EDGE('',*,*,#9231,.T.);
#13195=ORIENTED_EDGE('',*,*,#9232,.F.);
#13196=ORIENTED_EDGE('',*,*,#9233,.T.);
#13197=ORIENTED_EDGE('',*,*,#9229,.T.);
#13198=ORIENTED_EDGE('',*,*,#9234,.T.);
#13199=ORIENTED_EDGE('',*,*,#9235,.F.);
#13200=ORIENTED_EDGE('',*,*,#9236,.T.);
#13201=ORIENTED_EDGE('',*,*,#9232,.T.);
#13202=ORIENTED_EDGE('',*,*,#9237,.T.);
#13203=ORIENTED_EDGE('',*,*,#9238,.F.);
#13204=ORIENTED_EDGE('',*,*,#9239,.T.);
#13205=ORIENTED_EDGE('',*,*,#9235,.T.);
#13206=ORIENTED_EDGE('',*,*,#9240,.T.);
#13207=ORIENTED_EDGE('',*,*,#9241,.F.);
#13208=ORIENTED_EDGE('',*,*,#9242,.T.);
#13209=ORIENTED_EDGE('',*,*,#9238,.T.);
#13210=ORIENTED_EDGE('',*,*,#9243,.T.);
#13211=ORIENTED_EDGE('',*,*,#9244,.F.);
#13212=ORIENTED_EDGE('',*,*,#9245,.T.);
#13213=ORIENTED_EDGE('',*,*,#9246,.F.);
#13214=ORIENTED_EDGE('',*,*,#9247,.F.);
#13215=ORIENTED_EDGE('',*,*,#9248,.F.);
#13216=ORIENTED_EDGE('',*,*,#9249,.T.);
#13217=ORIENTED_EDGE('',*,*,#9244,.T.);
#13218=ORIENTED_EDGE('',*,*,#9250,.F.);
#13219=ORIENTED_EDGE('',*,*,#9251,.F.);
#13220=ORIENTED_EDGE('',*,*,#9252,.T.);
#13221=ORIENTED_EDGE('',*,*,#9248,.T.);
#13222=ORIENTED_EDGE('',*,*,#9253,.F.);
#13223=ORIENTED_EDGE('',*,*,#9254,.F.);
#13224=ORIENTED_EDGE('',*,*,#9255,.T.);
#13225=ORIENTED_EDGE('',*,*,#9251,.T.);
#13226=ORIENTED_EDGE('',*,*,#9256,.F.);
#13227=ORIENTED_EDGE('',*,*,#9257,.F.);
#13228=ORIENTED_EDGE('',*,*,#9258,.T.);
#13229=ORIENTED_EDGE('',*,*,#9254,.T.);
#13230=ORIENTED_EDGE('',*,*,#9259,.F.);
#13231=ORIENTED_EDGE('',*,*,#9260,.F.);
#13232=ORIENTED_EDGE('',*,*,#9261,.T.);
#13233=ORIENTED_EDGE('',*,*,#9257,.T.);
#13234=ORIENTED_EDGE('',*,*,#9262,.F.);
#13235=ORIENTED_EDGE('',*,*,#9263,.F.);
#13236=ORIENTED_EDGE('',*,*,#9264,.T.);
#13237=ORIENTED_EDGE('',*,*,#9260,.T.);
#13238=ORIENTED_EDGE('',*,*,#9265,.F.);
#13239=ORIENTED_EDGE('',*,*,#9266,.F.);
#13240=ORIENTED_EDGE('',*,*,#9267,.T.);
#13241=ORIENTED_EDGE('',*,*,#9263,.T.);
#13242=ORIENTED_EDGE('',*,*,#9268,.F.);
#13243=ORIENTED_EDGE('',*,*,#9269,.F.);
#13244=ORIENTED_EDGE('',*,*,#9270,.T.);
#13245=ORIENTED_EDGE('',*,*,#9266,.T.);
#13246=ORIENTED_EDGE('',*,*,#9271,.F.);
#13247=ORIENTED_EDGE('',*,*,#9272,.F.);
#13248=ORIENTED_EDGE('',*,*,#9273,.T.);
#13249=ORIENTED_EDGE('',*,*,#9269,.T.);
#13250=ORIENTED_EDGE('',*,*,#9274,.F.);
#13251=ORIENTED_EDGE('',*,*,#9275,.F.);
#13252=ORIENTED_EDGE('',*,*,#9276,.T.);
#13253=ORIENTED_EDGE('',*,*,#9272,.T.);
#13254=ORIENTED_EDGE('',*,*,#9277,.F.);
#13255=ORIENTED_EDGE('',*,*,#9278,.F.);
#13256=ORIENTED_EDGE('',*,*,#9279,.T.);
#13257=ORIENTED_EDGE('',*,*,#9275,.T.);
#13258=ORIENTED_EDGE('',*,*,#9280,.F.);
#13259=ORIENTED_EDGE('',*,*,#9281,.F.);
#13260=ORIENTED_EDGE('',*,*,#9282,.T.);
#13261=ORIENTED_EDGE('',*,*,#9278,.T.);
#13262=ORIENTED_EDGE('',*,*,#9283,.F.);
#13263=ORIENTED_EDGE('',*,*,#9284,.F.);
#13264=ORIENTED_EDGE('',*,*,#9285,.T.);
#13265=ORIENTED_EDGE('',*,*,#9281,.T.);
#13266=ORIENTED_EDGE('',*,*,#9286,.F.);
#13267=ORIENTED_EDGE('',*,*,#9287,.F.);
#13268=ORIENTED_EDGE('',*,*,#9288,.T.);
#13269=ORIENTED_EDGE('',*,*,#9284,.T.);
#13270=ORIENTED_EDGE('',*,*,#9289,.F.);
#13271=ORIENTED_EDGE('',*,*,#9290,.F.);
#13272=ORIENTED_EDGE('',*,*,#9291,.T.);
#13273=ORIENTED_EDGE('',*,*,#9287,.T.);
#13274=ORIENTED_EDGE('',*,*,#9292,.F.);
#13275=ORIENTED_EDGE('',*,*,#9293,.F.);
#13276=ORIENTED_EDGE('',*,*,#9294,.T.);
#13277=ORIENTED_EDGE('',*,*,#9290,.T.);
#13278=ORIENTED_EDGE('',*,*,#9295,.F.);
#13279=ORIENTED_EDGE('',*,*,#9296,.F.);
#13280=ORIENTED_EDGE('',*,*,#9297,.T.);
#13281=ORIENTED_EDGE('',*,*,#9293,.T.);
#13282=ORIENTED_EDGE('',*,*,#9298,.F.);
#13283=ORIENTED_EDGE('',*,*,#9299,.F.);
#13284=ORIENTED_EDGE('',*,*,#9300,.T.);
#13285=ORIENTED_EDGE('',*,*,#9296,.T.);
#13286=ORIENTED_EDGE('',*,*,#9301,.F.);
#13287=ORIENTED_EDGE('',*,*,#9302,.F.);
#13288=ORIENTED_EDGE('',*,*,#9303,.T.);
#13289=ORIENTED_EDGE('',*,*,#9299,.T.);
#13290=ORIENTED_EDGE('',*,*,#9304,.F.);
#13291=ORIENTED_EDGE('',*,*,#9305,.F.);
#13292=ORIENTED_EDGE('',*,*,#9306,.T.);
#13293=ORIENTED_EDGE('',*,*,#9302,.T.);
#13294=ORIENTED_EDGE('',*,*,#9307,.F.);
#13295=ORIENTED_EDGE('',*,*,#9308,.F.);
#13296=ORIENTED_EDGE('',*,*,#9309,.T.);
#13297=ORIENTED_EDGE('',*,*,#9305,.T.);
#13298=ORIENTED_EDGE('',*,*,#9310,.F.);
#13299=ORIENTED_EDGE('',*,*,#9246,.T.);
#13300=ORIENTED_EDGE('',*,*,#9311,.T.);
#13301=ORIENTED_EDGE('',*,*,#9312,.F.);
#13302=ORIENTED_EDGE('',*,*,#9313,.F.);
#13303=ORIENTED_EDGE('',*,*,#9314,.T.);
#13304=ORIENTED_EDGE('',*,*,#9314,.F.);
#13305=ORIENTED_EDGE('',*,*,#9315,.F.);
#13306=ORIENTED_EDGE('',*,*,#9243,.F.);
#13307=ORIENTED_EDGE('',*,*,#9240,.F.);
#13308=ORIENTED_EDGE('',*,*,#9237,.F.);
#13309=ORIENTED_EDGE('',*,*,#9234,.F.);
#13310=ORIENTED_EDGE('',*,*,#9231,.F.);
#13311=ORIENTED_EDGE('',*,*,#9228,.F.);
#13312=ORIENTED_EDGE('',*,*,#9225,.F.);
#13313=ORIENTED_EDGE('',*,*,#9222,.F.);
#13314=ORIENTED_EDGE('',*,*,#9219,.F.);
#13315=ORIENTED_EDGE('',*,*,#9216,.F.);
#13316=ORIENTED_EDGE('',*,*,#9213,.F.);
#13317=ORIENTED_EDGE('',*,*,#9210,.F.);
#13318=ORIENTED_EDGE('',*,*,#9207,.F.);
#13319=ORIENTED_EDGE('',*,*,#9204,.F.);
#13320=ORIENTED_EDGE('',*,*,#9201,.F.);
#13321=ORIENTED_EDGE('',*,*,#9198,.F.);
#13322=ORIENTED_EDGE('',*,*,#9195,.F.);
#13323=ORIENTED_EDGE('',*,*,#9192,.F.);
#13324=ORIENTED_EDGE('',*,*,#9189,.F.);
#13325=ORIENTED_EDGE('',*,*,#9186,.F.);
#13326=ORIENTED_EDGE('',*,*,#9183,.F.);
#13327=ORIENTED_EDGE('',*,*,#9180,.F.);
#13328=ORIENTED_EDGE('',*,*,#9316,.F.);
#13329=ORIENTED_EDGE('',*,*,#9317,.T.);
#13330=ORIENTED_EDGE('',*,*,#9310,.T.);
#13331=ORIENTED_EDGE('',*,*,#9307,.T.);
#13332=ORIENTED_EDGE('',*,*,#9304,.T.);
#13333=ORIENTED_EDGE('',*,*,#9301,.T.);
#13334=ORIENTED_EDGE('',*,*,#9298,.T.);
#13335=ORIENTED_EDGE('',*,*,#9295,.T.);
#13336=ORIENTED_EDGE('',*,*,#9292,.T.);
#13337=ORIENTED_EDGE('',*,*,#9289,.T.);
#13338=ORIENTED_EDGE('',*,*,#9286,.T.);
#13339=ORIENTED_EDGE('',*,*,#9283,.T.);
#13340=ORIENTED_EDGE('',*,*,#9280,.T.);
#13341=ORIENTED_EDGE('',*,*,#9277,.T.);
#13342=ORIENTED_EDGE('',*,*,#9274,.T.);
#13343=ORIENTED_EDGE('',*,*,#9271,.T.);
#13344=ORIENTED_EDGE('',*,*,#9268,.T.);
#13345=ORIENTED_EDGE('',*,*,#9265,.T.);
#13346=ORIENTED_EDGE('',*,*,#9262,.T.);
#13347=ORIENTED_EDGE('',*,*,#9259,.T.);
#13348=ORIENTED_EDGE('',*,*,#9256,.T.);
#13349=ORIENTED_EDGE('',*,*,#9253,.T.);
#13350=ORIENTED_EDGE('',*,*,#9250,.T.);
#13351=ORIENTED_EDGE('',*,*,#9247,.T.);
#13352=ORIENTED_EDGE('',*,*,#9318,.T.);
#13353=ORIENTED_EDGE('',*,*,#9319,.T.);
#13354=ORIENTED_EDGE('',*,*,#9320,.T.);
#13355=ORIENTED_EDGE('',*,*,#9321,.T.);
#13356=ORIENTED_EDGE('',*,*,#9316,.T.);
#13357=ORIENTED_EDGE('',*,*,#9308,.T.);
#13358=ORIENTED_EDGE('',*,*,#9317,.F.);
#13359=ORIENTED_EDGE('',*,*,#9321,.F.);
#13360=ORIENTED_EDGE('',*,*,#9322,.T.);
#13361=ORIENTED_EDGE('',*,*,#9311,.F.);
#13362=ORIENTED_EDGE('',*,*,#9245,.F.);
#13363=ORIENTED_EDGE('',*,*,#9249,.F.);
#13364=ORIENTED_EDGE('',*,*,#9252,.F.);
#13365=ORIENTED_EDGE('',*,*,#9255,.F.);
#13366=ORIENTED_EDGE('',*,*,#9258,.F.);
#13367=ORIENTED_EDGE('',*,*,#9261,.F.);
#13368=ORIENTED_EDGE('',*,*,#9264,.F.);
#13369=ORIENTED_EDGE('',*,*,#9267,.F.);
#13370=ORIENTED_EDGE('',*,*,#9270,.F.);
#13371=ORIENTED_EDGE('',*,*,#9273,.F.);
#13372=ORIENTED_EDGE('',*,*,#9276,.F.);
#13373=ORIENTED_EDGE('',*,*,#9279,.F.);
#13374=ORIENTED_EDGE('',*,*,#9282,.F.);
#13375=ORIENTED_EDGE('',*,*,#9285,.F.);
#13376=ORIENTED_EDGE('',*,*,#9288,.F.);
#13377=ORIENTED_EDGE('',*,*,#9291,.F.);
#13378=ORIENTED_EDGE('',*,*,#9294,.F.);
#13379=ORIENTED_EDGE('',*,*,#9297,.F.);
#13380=ORIENTED_EDGE('',*,*,#9300,.F.);
#13381=ORIENTED_EDGE('',*,*,#9303,.F.);
#13382=ORIENTED_EDGE('',*,*,#9306,.F.);
#13383=ORIENTED_EDGE('',*,*,#9309,.F.);
#13384=ORIENTED_EDGE('',*,*,#9322,.F.);
#13385=ORIENTED_EDGE('',*,*,#9320,.F.);
#13386=ORIENTED_EDGE('',*,*,#9178,.F.);
#13387=ORIENTED_EDGE('',*,*,#9182,.F.);
#13388=ORIENTED_EDGE('',*,*,#9185,.F.);
#13389=ORIENTED_EDGE('',*,*,#9188,.F.);
#13390=ORIENTED_EDGE('',*,*,#9191,.F.);
#13391=ORIENTED_EDGE('',*,*,#9194,.F.);
#13392=ORIENTED_EDGE('',*,*,#9197,.F.);
#13393=ORIENTED_EDGE('',*,*,#9200,.F.);
#13394=ORIENTED_EDGE('',*,*,#9203,.F.);
#13395=ORIENTED_EDGE('',*,*,#9206,.F.);
#13396=ORIENTED_EDGE('',*,*,#9209,.F.);
#13397=ORIENTED_EDGE('',*,*,#9212,.F.);
#13398=ORIENTED_EDGE('',*,*,#9215,.F.);
#13399=ORIENTED_EDGE('',*,*,#9218,.F.);
#13400=ORIENTED_EDGE('',*,*,#9221,.F.);
#13401=ORIENTED_EDGE('',*,*,#9224,.F.);
#13402=ORIENTED_EDGE('',*,*,#9227,.F.);
#13403=ORIENTED_EDGE('',*,*,#9230,.F.);
#13404=ORIENTED_EDGE('',*,*,#9233,.F.);
#13405=ORIENTED_EDGE('',*,*,#9236,.F.);
#13406=ORIENTED_EDGE('',*,*,#9239,.F.);
#13407=ORIENTED_EDGE('',*,*,#9242,.F.);
#13408=ORIENTED_EDGE('',*,*,#9323,.F.);
#13409=ORIENTED_EDGE('',*,*,#9313,.T.);
#13410=ORIENTED_EDGE('',*,*,#9324,.T.);
#13411=ORIENTED_EDGE('',*,*,#9325,.T.);
#13412=ORIENTED_EDGE('',*,*,#9324,.F.);
#13413=ORIENTED_EDGE('',*,*,#9312,.T.);
#13414=ORIENTED_EDGE('',*,*,#9326,.T.);
#13415=ORIENTED_EDGE('',*,*,#9241,.T.);
#13416=ORIENTED_EDGE('',*,*,#9315,.T.);
#13417=ORIENTED_EDGE('',*,*,#9326,.F.);
#13418=ORIENTED_EDGE('',*,*,#9323,.T.);
#13419=ORIENTED_EDGE('',*,*,#9327,.T.);
#13420=ORIENTED_EDGE('',*,*,#9328,.T.);
#13421=ORIENTED_EDGE('',*,*,#9329,.F.);
#13422=ORIENTED_EDGE('',*,*,#9330,.T.);
#13423=ORIENTED_EDGE('',*,*,#9331,.T.);
#13424=ORIENTED_EDGE('',*,*,#9332,.F.);
#13425=ORIENTED_EDGE('',*,*,#9333,.T.);
#13426=ORIENTED_EDGE('',*,*,#9334,.T.);
#13427=ORIENTED_EDGE('',*,*,#9335,.F.);
#13428=ORIENTED_EDGE('',*,*,#9336,.T.);
#13429=ORIENTED_EDGE('',*,*,#9337,.T.);
#13430=ORIENTED_EDGE('',*,*,#9338,.F.);
#13431=ORIENTED_EDGE('',*,*,#9339,.T.);
#13432=ORIENTED_EDGE('',*,*,#9340,.T.);
#13433=ORIENTED_EDGE('',*,*,#9341,.F.);
#13434=ORIENTED_EDGE('',*,*,#9342,.T.);
#13435=ORIENTED_EDGE('',*,*,#9343,.T.);
#13436=ORIENTED_EDGE('',*,*,#9344,.F.);
#13437=ORIENTED_EDGE('',*,*,#9345,.T.);
#13438=ORIENTED_EDGE('',*,*,#9346,.T.);
#13439=ORIENTED_EDGE('',*,*,#9347,.F.);
#13440=ORIENTED_EDGE('',*,*,#9348,.T.);
#13441=ORIENTED_EDGE('',*,*,#9349,.T.);
#13442=ORIENTED_EDGE('',*,*,#9350,.F.);
#13443=ORIENTED_EDGE('',*,*,#9351,.T.);
#13444=ORIENTED_EDGE('',*,*,#9352,.T.);
#13445=ORIENTED_EDGE('',*,*,#9353,.F.);
#13446=ORIENTED_EDGE('',*,*,#9354,.T.);
#13447=ORIENTED_EDGE('',*,*,#9355,.T.);
#13448=ORIENTED_EDGE('',*,*,#9356,.F.);
#13449=ORIENTED_EDGE('',*,*,#9357,.T.);
#13450=ORIENTED_EDGE('',*,*,#9358,.T.);
#13451=ORIENTED_EDGE('',*,*,#9359,.F.);
#13452=ORIENTED_EDGE('',*,*,#9360,.T.);
#13453=ORIENTED_EDGE('',*,*,#9361,.T.);
#13454=ORIENTED_EDGE('',*,*,#9362,.F.);
#13455=ORIENTED_EDGE('',*,*,#9363,.T.);
#13456=ORIENTED_EDGE('',*,*,#9364,.T.);
#13457=ORIENTED_EDGE('',*,*,#9365,.F.);
#13458=ORIENTED_EDGE('',*,*,#9366,.T.);
#13459=ORIENTED_EDGE('',*,*,#9367,.T.);
#13460=ORIENTED_EDGE('',*,*,#9368,.F.);
#13461=ORIENTED_EDGE('',*,*,#9369,.T.);
#13462=ORIENTED_EDGE('',*,*,#9370,.T.);
#13463=ORIENTED_EDGE('',*,*,#9371,.F.);
#13464=ORIENTED_EDGE('',*,*,#9372,.T.);
#13465=ORIENTED_EDGE('',*,*,#9373,.T.);
#13466=ORIENTED_EDGE('',*,*,#9374,.F.);
#13467=ORIENTED_EDGE('',*,*,#9375,.T.);
#13468=ORIENTED_EDGE('',*,*,#9376,.T.);
#13469=ORIENTED_EDGE('',*,*,#9377,.F.);
#13470=ORIENTED_EDGE('',*,*,#9378,.T.);
#13471=ORIENTED_EDGE('',*,*,#9379,.T.);
#13472=ORIENTED_EDGE('',*,*,#9380,.F.);
#13473=ORIENTED_EDGE('',*,*,#9381,.T.);
#13474=ORIENTED_EDGE('',*,*,#9382,.T.);
#13475=ORIENTED_EDGE('',*,*,#9383,.F.);
#13476=ORIENTED_EDGE('',*,*,#9384,.T.);
#13477=ORIENTED_EDGE('',*,*,#9385,.T.);
#13478=ORIENTED_EDGE('',*,*,#9386,.F.);
#13479=ORIENTED_EDGE('',*,*,#9387,.T.);
#13480=ORIENTED_EDGE('',*,*,#9388,.T.);
#13481=ORIENTED_EDGE('',*,*,#9389,.F.);
#13482=ORIENTED_EDGE('',*,*,#9390,.T.);
#13483=ORIENTED_EDGE('',*,*,#9391,.T.);
#13484=ORIENTED_EDGE('',*,*,#9392,.F.);
#13485=ORIENTED_EDGE('',*,*,#9393,.T.);
#13486=ORIENTED_EDGE('',*,*,#9394,.T.);
#13487=ORIENTED_EDGE('',*,*,#9395,.F.);
#13488=ORIENTED_EDGE('',*,*,#9396,.T.);
#13489=ORIENTED_EDGE('',*,*,#9397,.T.);
#13490=ORIENTED_EDGE('',*,*,#9398,.F.);
#13491=ORIENTED_EDGE('',*,*,#9399,.T.);
#13492=ORIENTED_EDGE('',*,*,#9400,.T.);
#13493=ORIENTED_EDGE('',*,*,#9401,.F.);
#13494=ORIENTED_EDGE('',*,*,#9402,.T.);
#13495=ORIENTED_EDGE('',*,*,#9403,.T.);
#13496=ORIENTED_EDGE('',*,*,#9404,.F.);
#13497=ORIENTED_EDGE('',*,*,#9405,.T.);
#13498=ORIENTED_EDGE('',*,*,#9406,.T.);
#13499=ORIENTED_EDGE('',*,*,#9407,.F.);
#13500=ORIENTED_EDGE('',*,*,#9408,.T.);
#13501=ORIENTED_EDGE('',*,*,#9409,.T.);
#13502=ORIENTED_EDGE('',*,*,#9410,.F.);
#13503=ORIENTED_EDGE('',*,*,#9411,.T.);
#13504=ORIENTED_EDGE('',*,*,#9412,.T.);
#13505=ORIENTED_EDGE('',*,*,#9413,.F.);
#13506=ORIENTED_EDGE('',*,*,#9414,.T.);
#13507=ORIENTED_EDGE('',*,*,#9415,.T.);
#13508=ORIENTED_EDGE('',*,*,#9416,.F.);
#13509=ORIENTED_EDGE('',*,*,#9417,.T.);
#13510=ORIENTED_EDGE('',*,*,#9418,.T.);
#13511=ORIENTED_EDGE('',*,*,#9419,.F.);
#13512=ORIENTED_EDGE('',*,*,#9420,.T.);
#13513=ORIENTED_EDGE('',*,*,#9421,.T.);
#13514=ORIENTED_EDGE('',*,*,#9422,.F.);
#13515=ORIENTED_EDGE('',*,*,#9423,.T.);
#13516=ORIENTED_EDGE('',*,*,#9424,.T.);
#13517=ORIENTED_EDGE('',*,*,#9425,.F.);
#13518=ORIENTED_EDGE('',*,*,#9426,.T.);
#13519=ORIENTED_EDGE('',*,*,#9427,.T.);
#13520=ORIENTED_EDGE('',*,*,#9428,.F.);
#13521=ORIENTED_EDGE('',*,*,#9429,.T.);
#13522=ORIENTED_EDGE('',*,*,#9430,.T.);
#13523=ORIENTED_EDGE('',*,*,#9431,.F.);
#13524=ORIENTED_EDGE('',*,*,#9432,.T.);
#13525=ORIENTED_EDGE('',*,*,#9433,.T.);
#13526=ORIENTED_EDGE('',*,*,#9434,.F.);
#13527=ORIENTED_EDGE('',*,*,#9325,.F.);
#13528=ORIENTED_EDGE('',*,*,#9435,.F.);
#13529=ORIENTED_EDGE('',*,*,#9436,.F.);
#13530=ORIENTED_EDGE('',*,*,#9437,.F.);
#13531=ORIENTED_EDGE('',*,*,#9438,.F.);
#13532=ORIENTED_EDGE('',*,*,#9439,.F.);
#13533=ORIENTED_EDGE('',*,*,#9440,.F.);
#13534=ORIENTED_EDGE('',*,*,#9441,.F.);
#13535=ORIENTED_EDGE('',*,*,#9442,.F.);
#13536=ORIENTED_EDGE('',*,*,#9443,.F.);
#13537=ORIENTED_EDGE('',*,*,#9444,.F.);
#13538=ORIENTED_EDGE('',*,*,#9445,.F.);
#13539=ORIENTED_EDGE('',*,*,#9446,.F.);
#13540=ORIENTED_EDGE('',*,*,#9447,.T.);
#13541=ORIENTED_EDGE('',*,*,#9448,.F.);
#13542=ORIENTED_EDGE('',*,*,#9449,.F.);
#13543=ORIENTED_EDGE('',*,*,#9438,.T.);
#13544=ORIENTED_EDGE('',*,*,#9450,.F.);
#13545=ORIENTED_EDGE('',*,*,#9451,.F.);
#13546=ORIENTED_EDGE('',*,*,#9452,.F.);
#13547=ORIENTED_EDGE('',*,*,#9436,.T.);
#13548=ORIENTED_EDGE('',*,*,#9453,.F.);
#13549=ORIENTED_EDGE('',*,*,#9454,.F.);
#13550=ORIENTED_EDGE('',*,*,#9455,.F.);
#13551=ORIENTED_EDGE('',*,*,#9446,.T.);
#13552=ORIENTED_EDGE('',*,*,#9456,.F.);
#13553=ORIENTED_EDGE('',*,*,#9457,.F.);
#13554=ORIENTED_EDGE('',*,*,#9458,.F.);
#13555=ORIENTED_EDGE('',*,*,#9444,.T.);
#13556=ORIENTED_EDGE('',*,*,#9459,.F.);
#13557=ORIENTED_EDGE('',*,*,#9460,.F.);
#13558=ORIENTED_EDGE('',*,*,#9461,.F.);
#13559=ORIENTED_EDGE('',*,*,#9442,.T.);
#13560=ORIENTED_EDGE('',*,*,#9462,.F.);
#13561=ORIENTED_EDGE('',*,*,#9463,.F.);
#13562=ORIENTED_EDGE('',*,*,#9464,.F.);
#13563=ORIENTED_EDGE('',*,*,#9440,.T.);
#13564=ORIENTED_EDGE('',*,*,#9465,.F.);
#13565=ORIENTED_EDGE('',*,*,#9466,.F.);
#13566=ORIENTED_EDGE('',*,*,#9447,.F.);
#13567=ORIENTED_EDGE('',*,*,#9439,.T.);
#13568=ORIENTED_EDGE('',*,*,#9467,.F.);
#13569=ORIENTED_EDGE('',*,*,#9468,.F.);
#13570=ORIENTED_EDGE('',*,*,#9469,.T.);
#13571=ORIENTED_EDGE('',*,*,#9465,.T.);
#13572=ORIENTED_EDGE('',*,*,#9470,.T.);
#13573=ORIENTED_EDGE('',*,*,#9471,.T.);
#13574=ORIENTED_EDGE('',*,*,#9441,.T.);
#13575=ORIENTED_EDGE('',*,*,#9472,.F.);
#13576=ORIENTED_EDGE('',*,*,#9473,.F.);
#13577=ORIENTED_EDGE('',*,*,#9467,.T.);
#13578=ORIENTED_EDGE('',*,*,#9461,.T.);
#13579=ORIENTED_EDGE('',*,*,#9474,.T.);
#13580=ORIENTED_EDGE('',*,*,#9475,.F.);
#13581=ORIENTED_EDGE('',*,*,#9462,.T.);
#13582=ORIENTED_EDGE('',*,*,#9476,.T.);
#13583=ORIENTED_EDGE('',*,*,#9477,.T.);
#13584=ORIENTED_EDGE('',*,*,#9437,.T.);
#13585=ORIENTED_EDGE('',*,*,#9469,.F.);
#13586=ORIENTED_EDGE('',*,*,#9478,.F.);
#13587=ORIENTED_EDGE('',*,*,#9479,.T.);
#13588=ORIENTED_EDGE('',*,*,#9450,.T.);
#13589=ORIENTED_EDGE('',*,*,#9480,.T.);
#13590=ORIENTED_EDGE('',*,*,#9481,.T.);
#13591=ORIENTED_EDGE('',*,*,#9443,.T.);
#13592=ORIENTED_EDGE('',*,*,#9482,.F.);
#13593=ORIENTED_EDGE('',*,*,#9483,.F.);
#13594=ORIENTED_EDGE('',*,*,#9472,.T.);
#13595=ORIENTED_EDGE('',*,*,#9458,.T.);
#13596=ORIENTED_EDGE('',*,*,#9484,.T.);
#13597=ORIENTED_EDGE('',*,*,#9485,.F.);
#13598=ORIENTED_EDGE('',*,*,#9459,.T.);
#13599=ORIENTED_EDGE('',*,*,#9475,.T.);
#13600=ORIENTED_EDGE('',*,*,#9486,.T.);
#13601=ORIENTED_EDGE('',*,*,#9463,.T.);
#13602=ORIENTED_EDGE('',*,*,#9477,.F.);
#13603=ORIENTED_EDGE('',*,*,#9487,.F.);
#13604=ORIENTED_EDGE('',*,*,#9460,.T.);
#13605=ORIENTED_EDGE('',*,*,#9486,.F.);
#13606=ORIENTED_EDGE('',*,*,#9474,.F.);
#13607=ORIENTED_EDGE('',*,*,#9457,.T.);
#13608=ORIENTED_EDGE('',*,*,#9488,.F.);
#13609=ORIENTED_EDGE('',*,*,#9484,.F.);
#13610=ORIENTED_EDGE('',*,*,#9454,.T.);
#13611=ORIENTED_EDGE('',*,*,#9489,.F.);
#13612=ORIENTED_EDGE('',*,*,#9490,.F.);
#13613=ORIENTED_EDGE('',*,*,#9451,.T.);
#13614=ORIENTED_EDGE('',*,*,#9481,.F.);
#13615=ORIENTED_EDGE('',*,*,#9491,.F.);
#13616=ORIENTED_EDGE('',*,*,#9448,.T.);
#13617=ORIENTED_EDGE('',*,*,#9466,.T.);
#13618=ORIENTED_EDGE('',*,*,#9471,.F.);
#13619=ORIENTED_EDGE('',*,*,#9492,.F.);
#13620=ORIENTED_EDGE('',*,*,#9445,.T.);
#13621=ORIENTED_EDGE('',*,*,#9493,.F.);
#13622=ORIENTED_EDGE('',*,*,#9494,.F.);
#13623=ORIENTED_EDGE('',*,*,#9482,.T.);
#13624=ORIENTED_EDGE('',*,*,#9455,.T.);
#13625=ORIENTED_EDGE('',*,*,#9490,.T.);
#13626=ORIENTED_EDGE('',*,*,#9495,.F.);
#13627=ORIENTED_EDGE('',*,*,#9456,.T.);
#13628=ORIENTED_EDGE('',*,*,#9485,.T.);
#13629=ORIENTED_EDGE('',*,*,#9488,.T.);
#13630=ORIENTED_EDGE('',*,*,#9453,.T.);
#13631=ORIENTED_EDGE('',*,*,#9495,.T.);
#13632=ORIENTED_EDGE('',*,*,#9489,.T.);
#13633=ORIENTED_EDGE('',*,*,#9435,.T.);
#13634=ORIENTED_EDGE('',*,*,#9479,.F.);
#13635=ORIENTED_EDGE('',*,*,#9496,.F.);
#13636=ORIENTED_EDGE('',*,*,#9493,.T.);
#13637=ORIENTED_EDGE('',*,*,#9464,.T.);
#13638=ORIENTED_EDGE('',*,*,#9487,.T.);
#13639=ORIENTED_EDGE('',*,*,#9476,.F.);
#13640=ORIENTED_EDGE('',*,*,#9449,.T.);
#13641=ORIENTED_EDGE('',*,*,#9492,.T.);
#13642=ORIENTED_EDGE('',*,*,#9470,.F.);
#13643=ORIENTED_EDGE('',*,*,#9452,.T.);
#13644=ORIENTED_EDGE('',*,*,#9491,.T.);
#13645=ORIENTED_EDGE('',*,*,#9480,.F.);
#13646=ORIENTED_EDGE('',*,*,#9497,.F.);
#13647=ORIENTED_EDGE('',*,*,#9498,.T.);
#13648=ORIENTED_EDGE('',*,*,#9327,.F.);
#13649=ORIENTED_EDGE('',*,*,#9499,.F.);
#13650=ORIENTED_EDGE('',*,*,#9500,.F.);
#13651=ORIENTED_EDGE('',*,*,#9501,.F.);
#13652=ORIENTED_EDGE('',*,*,#9328,.F.);
#13653=ORIENTED_EDGE('',*,*,#9498,.F.);
#13654=ORIENTED_EDGE('',*,*,#9502,.F.);
#13655=ORIENTED_EDGE('',*,*,#9503,.T.);
#13656=ORIENTED_EDGE('',*,*,#9333,.F.);
#13657=ORIENTED_EDGE('',*,*,#9504,.F.);
#13658=ORIENTED_EDGE('',*,*,#9505,.F.);
#13659=ORIENTED_EDGE('',*,*,#9506,.F.);
#13660=ORIENTED_EDGE('',*,*,#9334,.F.);
#13661=ORIENTED_EDGE('',*,*,#9503,.F.);
#13662=ORIENTED_EDGE('',*,*,#9507,.F.);
#13663=ORIENTED_EDGE('',*,*,#9508,.T.);
#13664=ORIENTED_EDGE('',*,*,#9339,.F.);
#13665=ORIENTED_EDGE('',*,*,#9509,.F.);
#13666=ORIENTED_EDGE('',*,*,#9510,.F.);
#13667=ORIENTED_EDGE('',*,*,#9511,.F.);
#13668=ORIENTED_EDGE('',*,*,#9340,.F.);
#13669=ORIENTED_EDGE('',*,*,#9508,.F.);
#13670=ORIENTED_EDGE('',*,*,#9512,.F.);
#13671=ORIENTED_EDGE('',*,*,#9513,.T.);
#13672=ORIENTED_EDGE('',*,*,#9345,.F.);
#13673=ORIENTED_EDGE('',*,*,#9514,.F.);
#13674=ORIENTED_EDGE('',*,*,#9515,.F.);
#13675=ORIENTED_EDGE('',*,*,#9516,.F.);
#13676=ORIENTED_EDGE('',*,*,#9346,.F.);
#13677=ORIENTED_EDGE('',*,*,#9513,.F.);
#13678=ORIENTED_EDGE('',*,*,#9517,.F.);
#13679=ORIENTED_EDGE('',*,*,#9518,.T.);
#13680=ORIENTED_EDGE('',*,*,#9351,.F.);
#13681=ORIENTED_EDGE('',*,*,#9519,.F.);
#13682=ORIENTED_EDGE('',*,*,#9520,.F.);
#13683=ORIENTED_EDGE('',*,*,#9521,.F.);
#13684=ORIENTED_EDGE('',*,*,#9352,.F.);
#13685=ORIENTED_EDGE('',*,*,#9518,.F.);
#13686=ORIENTED_EDGE('',*,*,#9522,.F.);
#13687=ORIENTED_EDGE('',*,*,#9523,.T.);
#13688=ORIENTED_EDGE('',*,*,#9357,.F.);
#13689=ORIENTED_EDGE('',*,*,#9524,.F.);
#13690=ORIENTED_EDGE('',*,*,#9525,.F.);
#13691=ORIENTED_EDGE('',*,*,#9526,.F.);
#13692=ORIENTED_EDGE('',*,*,#9358,.F.);
#13693=ORIENTED_EDGE('',*,*,#9523,.F.);
#13694=ORIENTED_EDGE('',*,*,#9527,.F.);
#13695=ORIENTED_EDGE('',*,*,#9528,.T.);
#13696=ORIENTED_EDGE('',*,*,#9363,.F.);
#13697=ORIENTED_EDGE('',*,*,#9529,.F.);
#13698=ORIENTED_EDGE('',*,*,#9530,.F.);
#13699=ORIENTED_EDGE('',*,*,#9531,.F.);
#13700=ORIENTED_EDGE('',*,*,#9364,.F.);
#13701=ORIENTED_EDGE('',*,*,#9528,.F.);
#13702=ORIENTED_EDGE('',*,*,#9532,.F.);
#13703=ORIENTED_EDGE('',*,*,#9533,.T.);
#13704=ORIENTED_EDGE('',*,*,#9369,.F.);
#13705=ORIENTED_EDGE('',*,*,#9534,.F.);
#13706=ORIENTED_EDGE('',*,*,#9535,.F.);
#13707=ORIENTED_EDGE('',*,*,#9536,.F.);
#13708=ORIENTED_EDGE('',*,*,#9370,.F.);
#13709=ORIENTED_EDGE('',*,*,#9533,.F.);
#13710=ORIENTED_EDGE('',*,*,#9537,.F.);
#13711=ORIENTED_EDGE('',*,*,#9538,.T.);
#13712=ORIENTED_EDGE('',*,*,#9375,.F.);
#13713=ORIENTED_EDGE('',*,*,#9539,.F.);
#13714=ORIENTED_EDGE('',*,*,#9540,.F.);
#13715=ORIENTED_EDGE('',*,*,#9541,.F.);
#13716=ORIENTED_EDGE('',*,*,#9376,.F.);
#13717=ORIENTED_EDGE('',*,*,#9538,.F.);
#13718=ORIENTED_EDGE('',*,*,#9542,.F.);
#13719=ORIENTED_EDGE('',*,*,#9543,.T.);
#13720=ORIENTED_EDGE('',*,*,#9378,.F.);
#13721=ORIENTED_EDGE('',*,*,#9544,.F.);
#13722=ORIENTED_EDGE('',*,*,#9545,.F.);
#13723=ORIENTED_EDGE('',*,*,#9546,.F.);
#13724=ORIENTED_EDGE('',*,*,#9379,.F.);
#13725=ORIENTED_EDGE('',*,*,#9543,.F.);
#13726=ORIENTED_EDGE('',*,*,#9547,.F.);
#13727=ORIENTED_EDGE('',*,*,#9548,.T.);
#13728=ORIENTED_EDGE('',*,*,#9384,.F.);
#13729=ORIENTED_EDGE('',*,*,#9549,.F.);
#13730=ORIENTED_EDGE('',*,*,#9550,.F.);
#13731=ORIENTED_EDGE('',*,*,#9551,.F.);
#13732=ORIENTED_EDGE('',*,*,#9385,.F.);
#13733=ORIENTED_EDGE('',*,*,#9548,.F.);
#13734=ORIENTED_EDGE('',*,*,#9552,.F.);
#13735=ORIENTED_EDGE('',*,*,#9553,.T.);
#13736=ORIENTED_EDGE('',*,*,#9390,.F.);
#13737=ORIENTED_EDGE('',*,*,#9554,.F.);
#13738=ORIENTED_EDGE('',*,*,#9555,.F.);
#13739=ORIENTED_EDGE('',*,*,#9556,.F.);
#13740=ORIENTED_EDGE('',*,*,#9391,.F.);
#13741=ORIENTED_EDGE('',*,*,#9553,.F.);
#13742=ORIENTED_EDGE('',*,*,#9557,.F.);
#13743=ORIENTED_EDGE('',*,*,#9558,.T.);
#13744=ORIENTED_EDGE('',*,*,#9396,.F.);
#13745=ORIENTED_EDGE('',*,*,#9559,.F.);
#13746=ORIENTED_EDGE('',*,*,#9560,.F.);
#13747=ORIENTED_EDGE('',*,*,#9561,.F.);
#13748=ORIENTED_EDGE('',*,*,#9397,.F.);
#13749=ORIENTED_EDGE('',*,*,#9558,.F.);
#13750=ORIENTED_EDGE('',*,*,#9562,.F.);
#13751=ORIENTED_EDGE('',*,*,#9563,.T.);
#13752=ORIENTED_EDGE('',*,*,#9402,.F.);
#13753=ORIENTED_EDGE('',*,*,#9564,.F.);
#13754=ORIENTED_EDGE('',*,*,#9565,.F.);
#13755=ORIENTED_EDGE('',*,*,#9566,.F.);
#13756=ORIENTED_EDGE('',*,*,#9403,.F.);
#13757=ORIENTED_EDGE('',*,*,#9563,.F.);
#13758=ORIENTED_EDGE('',*,*,#9567,.F.);
#13759=ORIENTED_EDGE('',*,*,#9568,.T.);
#13760=ORIENTED_EDGE('',*,*,#9408,.F.);
#13761=ORIENTED_EDGE('',*,*,#9569,.F.);
#13762=ORIENTED_EDGE('',*,*,#9570,.F.);
#13763=ORIENTED_EDGE('',*,*,#9571,.F.);
#13764=ORIENTED_EDGE('',*,*,#9409,.F.);
#13765=ORIENTED_EDGE('',*,*,#9568,.F.);
#13766=ORIENTED_EDGE('',*,*,#9572,.F.);
#13767=ORIENTED_EDGE('',*,*,#9573,.T.);
#13768=ORIENTED_EDGE('',*,*,#9414,.F.);
#13769=ORIENTED_EDGE('',*,*,#9574,.F.);
#13770=ORIENTED_EDGE('',*,*,#9575,.F.);
#13771=ORIENTED_EDGE('',*,*,#9576,.F.);
#13772=ORIENTED_EDGE('',*,*,#9415,.F.);
#13773=ORIENTED_EDGE('',*,*,#9573,.F.);
#13774=ORIENTED_EDGE('',*,*,#9577,.F.);
#13775=ORIENTED_EDGE('',*,*,#9578,.T.);
#13776=ORIENTED_EDGE('',*,*,#9420,.F.);
#13777=ORIENTED_EDGE('',*,*,#9579,.F.);
#13778=ORIENTED_EDGE('',*,*,#9580,.F.);
#13779=ORIENTED_EDGE('',*,*,#9581,.F.);
#13780=ORIENTED_EDGE('',*,*,#9421,.F.);
#13781=ORIENTED_EDGE('',*,*,#9578,.F.);
#13782=ORIENTED_EDGE('',*,*,#9582,.F.);
#13783=ORIENTED_EDGE('',*,*,#9583,.T.);
#13784=ORIENTED_EDGE('',*,*,#9426,.F.);
#13785=ORIENTED_EDGE('',*,*,#9584,.F.);
#13786=ORIENTED_EDGE('',*,*,#9585,.F.);
#13787=ORIENTED_EDGE('',*,*,#9586,.F.);
#13788=ORIENTED_EDGE('',*,*,#9427,.F.);
#13789=ORIENTED_EDGE('',*,*,#9583,.F.);
#13790=ORIENTED_EDGE('',*,*,#9587,.F.);
#13791=ORIENTED_EDGE('',*,*,#9588,.T.);
#13792=ORIENTED_EDGE('',*,*,#9423,.F.);
#13793=ORIENTED_EDGE('',*,*,#9589,.F.);
#13794=ORIENTED_EDGE('',*,*,#9590,.F.);
#13795=ORIENTED_EDGE('',*,*,#9591,.F.);
#13796=ORIENTED_EDGE('',*,*,#9424,.F.);
#13797=ORIENTED_EDGE('',*,*,#9588,.F.);
#13798=ORIENTED_EDGE('',*,*,#9592,.F.);
#13799=ORIENTED_EDGE('',*,*,#9593,.T.);
#13800=ORIENTED_EDGE('',*,*,#9417,.F.);
#13801=ORIENTED_EDGE('',*,*,#9594,.F.);
#13802=ORIENTED_EDGE('',*,*,#9595,.F.);
#13803=ORIENTED_EDGE('',*,*,#9596,.F.);
#13804=ORIENTED_EDGE('',*,*,#9418,.F.);
#13805=ORIENTED_EDGE('',*,*,#9593,.F.);
#13806=ORIENTED_EDGE('',*,*,#9597,.F.);
#13807=ORIENTED_EDGE('',*,*,#9598,.T.);
#13808=ORIENTED_EDGE('',*,*,#9411,.F.);
#13809=ORIENTED_EDGE('',*,*,#9599,.F.);
#13810=ORIENTED_EDGE('',*,*,#9600,.F.);
#13811=ORIENTED_EDGE('',*,*,#9601,.F.);
#13812=ORIENTED_EDGE('',*,*,#9412,.F.);
#13813=ORIENTED_EDGE('',*,*,#9598,.F.);
#13814=ORIENTED_EDGE('',*,*,#9602,.F.);
#13815=ORIENTED_EDGE('',*,*,#9603,.T.);
#13816=ORIENTED_EDGE('',*,*,#9405,.F.);
#13817=ORIENTED_EDGE('',*,*,#9604,.F.);
#13818=ORIENTED_EDGE('',*,*,#9605,.F.);
#13819=ORIENTED_EDGE('',*,*,#9606,.F.);
#13820=ORIENTED_EDGE('',*,*,#9406,.F.);
#13821=ORIENTED_EDGE('',*,*,#9603,.F.);
#13822=ORIENTED_EDGE('',*,*,#9607,.F.);
#13823=ORIENTED_EDGE('',*,*,#9608,.T.);
#13824=ORIENTED_EDGE('',*,*,#9399,.F.);
#13825=ORIENTED_EDGE('',*,*,#9609,.F.);
#13826=ORIENTED_EDGE('',*,*,#9610,.F.);
#13827=ORIENTED_EDGE('',*,*,#9611,.F.);
#13828=ORIENTED_EDGE('',*,*,#9400,.F.);
#13829=ORIENTED_EDGE('',*,*,#9608,.F.);
#13830=ORIENTED_EDGE('',*,*,#9612,.F.);
#13831=ORIENTED_EDGE('',*,*,#9613,.T.);
#13832=ORIENTED_EDGE('',*,*,#9393,.F.);
#13833=ORIENTED_EDGE('',*,*,#9614,.F.);
#13834=ORIENTED_EDGE('',*,*,#9615,.F.);
#13835=ORIENTED_EDGE('',*,*,#9616,.F.);
#13836=ORIENTED_EDGE('',*,*,#9394,.F.);
#13837=ORIENTED_EDGE('',*,*,#9613,.F.);
#13838=ORIENTED_EDGE('',*,*,#9617,.F.);
#13839=ORIENTED_EDGE('',*,*,#9618,.T.);
#13840=ORIENTED_EDGE('',*,*,#9387,.F.);
#13841=ORIENTED_EDGE('',*,*,#9619,.F.);
#13842=ORIENTED_EDGE('',*,*,#9620,.F.);
#13843=ORIENTED_EDGE('',*,*,#9621,.F.);
#13844=ORIENTED_EDGE('',*,*,#9388,.F.);
#13845=ORIENTED_EDGE('',*,*,#9618,.F.);
#13846=ORIENTED_EDGE('',*,*,#9622,.F.);
#13847=ORIENTED_EDGE('',*,*,#9623,.T.);
#13848=ORIENTED_EDGE('',*,*,#9381,.F.);
#13849=ORIENTED_EDGE('',*,*,#9624,.F.);
#13850=ORIENTED_EDGE('',*,*,#9625,.F.);
#13851=ORIENTED_EDGE('',*,*,#9626,.F.);
#13852=ORIENTED_EDGE('',*,*,#9382,.F.);
#13853=ORIENTED_EDGE('',*,*,#9623,.F.);
#13854=ORIENTED_EDGE('',*,*,#9627,.F.);
#13855=ORIENTED_EDGE('',*,*,#9628,.T.);
#13856=ORIENTED_EDGE('',*,*,#9429,.F.);
#13857=ORIENTED_EDGE('',*,*,#9629,.F.);
#13858=ORIENTED_EDGE('',*,*,#9630,.F.);
#13859=ORIENTED_EDGE('',*,*,#9631,.F.);
#13860=ORIENTED_EDGE('',*,*,#9430,.F.);
#13861=ORIENTED_EDGE('',*,*,#9628,.F.);
#13862=ORIENTED_EDGE('',*,*,#9632,.F.);
#13863=ORIENTED_EDGE('',*,*,#9633,.T.);
#13864=ORIENTED_EDGE('',*,*,#9372,.F.);
#13865=ORIENTED_EDGE('',*,*,#9634,.F.);
#13866=ORIENTED_EDGE('',*,*,#9635,.F.);
#13867=ORIENTED_EDGE('',*,*,#9636,.F.);
#13868=ORIENTED_EDGE('',*,*,#9373,.F.);
#13869=ORIENTED_EDGE('',*,*,#9633,.F.);
#13870=ORIENTED_EDGE('',*,*,#9637,.F.);
#13871=ORIENTED_EDGE('',*,*,#9638,.T.);
#13872=ORIENTED_EDGE('',*,*,#9366,.F.);
#13873=ORIENTED_EDGE('',*,*,#9639,.F.);
#13874=ORIENTED_EDGE('',*,*,#9640,.F.);
#13875=ORIENTED_EDGE('',*,*,#9641,.F.);
#13876=ORIENTED_EDGE('',*,*,#9367,.F.);
#13877=ORIENTED_EDGE('',*,*,#9638,.F.);
#13878=ORIENTED_EDGE('',*,*,#9642,.F.);
#13879=ORIENTED_EDGE('',*,*,#9643,.T.);
#13880=ORIENTED_EDGE('',*,*,#9360,.F.);
#13881=ORIENTED_EDGE('',*,*,#9644,.F.);
#13882=ORIENTED_EDGE('',*,*,#9645,.F.);
#13883=ORIENTED_EDGE('',*,*,#9646,.F.);
#13884=ORIENTED_EDGE('',*,*,#9361,.F.);
#13885=ORIENTED_EDGE('',*,*,#9643,.F.);
#13886=ORIENTED_EDGE('',*,*,#9647,.F.);
#13887=ORIENTED_EDGE('',*,*,#9648,.T.);
#13888=ORIENTED_EDGE('',*,*,#9354,.F.);
#13889=ORIENTED_EDGE('',*,*,#9649,.F.);
#13890=ORIENTED_EDGE('',*,*,#9650,.F.);
#13891=ORIENTED_EDGE('',*,*,#9651,.F.);
#13892=ORIENTED_EDGE('',*,*,#9355,.F.);
#13893=ORIENTED_EDGE('',*,*,#9648,.F.);
#13894=ORIENTED_EDGE('',*,*,#9652,.F.);
#13895=ORIENTED_EDGE('',*,*,#9653,.T.);
#13896=ORIENTED_EDGE('',*,*,#9348,.F.);
#13897=ORIENTED_EDGE('',*,*,#9654,.F.);
#13898=ORIENTED_EDGE('',*,*,#9655,.F.);
#13899=ORIENTED_EDGE('',*,*,#9656,.F.);
#13900=ORIENTED_EDGE('',*,*,#9349,.F.);
#13901=ORIENTED_EDGE('',*,*,#9653,.F.);
#13902=ORIENTED_EDGE('',*,*,#9657,.F.);
#13903=ORIENTED_EDGE('',*,*,#9658,.T.);
#13904=ORIENTED_EDGE('',*,*,#9342,.F.);
#13905=ORIENTED_EDGE('',*,*,#9659,.F.);
#13906=ORIENTED_EDGE('',*,*,#9660,.F.);
#13907=ORIENTED_EDGE('',*,*,#9661,.F.);
#13908=ORIENTED_EDGE('',*,*,#9343,.F.);
#13909=ORIENTED_EDGE('',*,*,#9658,.F.);
#13910=ORIENTED_EDGE('',*,*,#9662,.F.);
#13911=ORIENTED_EDGE('',*,*,#9663,.T.);
#13912=ORIENTED_EDGE('',*,*,#9336,.F.);
#13913=ORIENTED_EDGE('',*,*,#9664,.F.);
#13914=ORIENTED_EDGE('',*,*,#9665,.F.);
#13915=ORIENTED_EDGE('',*,*,#9666,.F.);
#13916=ORIENTED_EDGE('',*,*,#9337,.F.);
#13917=ORIENTED_EDGE('',*,*,#9663,.F.);
#13918=ORIENTED_EDGE('',*,*,#9667,.F.);
#13919=ORIENTED_EDGE('',*,*,#9668,.T.);
#13920=ORIENTED_EDGE('',*,*,#9330,.F.);
#13921=ORIENTED_EDGE('',*,*,#9669,.F.);
#13922=ORIENTED_EDGE('',*,*,#9670,.F.);
#13923=ORIENTED_EDGE('',*,*,#9671,.F.);
#13924=ORIENTED_EDGE('',*,*,#9331,.F.);
#13925=ORIENTED_EDGE('',*,*,#9668,.F.);
#13926=ORIENTED_EDGE('',*,*,#9672,.F.);
#13927=ORIENTED_EDGE('',*,*,#9673,.T.);
#13928=ORIENTED_EDGE('',*,*,#9432,.F.);
#13929=ORIENTED_EDGE('',*,*,#9674,.F.);
#13930=ORIENTED_EDGE('',*,*,#9675,.F.);
#13931=ORIENTED_EDGE('',*,*,#9676,.F.);
#13932=ORIENTED_EDGE('',*,*,#9433,.F.);
#13933=ORIENTED_EDGE('',*,*,#9673,.F.);
#13934=ORIENTED_EDGE('',*,*,#9631,.T.);
#13935=ORIENTED_EDGE('',*,*,#9677,.F.);
#13936=ORIENTED_EDGE('',*,*,#9674,.T.);
#13937=ORIENTED_EDGE('',*,*,#9431,.T.);
#13938=ORIENTED_EDGE('',*,*,#9586,.T.);
#13939=ORIENTED_EDGE('',*,*,#9678,.F.);
#13940=ORIENTED_EDGE('',*,*,#9629,.T.);
#13941=ORIENTED_EDGE('',*,*,#9428,.T.);
#13942=ORIENTED_EDGE('',*,*,#9584,.T.);
#13943=ORIENTED_EDGE('',*,*,#9425,.T.);
#13944=ORIENTED_EDGE('',*,*,#9591,.T.);
#13945=ORIENTED_EDGE('',*,*,#9679,.F.);
#13946=ORIENTED_EDGE('',*,*,#9581,.T.);
#13947=ORIENTED_EDGE('',*,*,#9680,.F.);
#13948=ORIENTED_EDGE('',*,*,#9589,.T.);
#13949=ORIENTED_EDGE('',*,*,#9422,.T.);
#13950=ORIENTED_EDGE('',*,*,#9579,.T.);
#13951=ORIENTED_EDGE('',*,*,#9419,.T.);
#13952=ORIENTED_EDGE('',*,*,#9596,.T.);
#13953=ORIENTED_EDGE('',*,*,#9681,.F.);
#13954=ORIENTED_EDGE('',*,*,#9576,.T.);
#13955=ORIENTED_EDGE('',*,*,#9682,.F.);
#13956=ORIENTED_EDGE('',*,*,#9594,.T.);
#13957=ORIENTED_EDGE('',*,*,#9416,.T.);
#13958=ORIENTED_EDGE('',*,*,#9574,.T.);
#13959=ORIENTED_EDGE('',*,*,#9413,.T.);
#13960=ORIENTED_EDGE('',*,*,#9601,.T.);
#13961=ORIENTED_EDGE('',*,*,#9683,.F.);
#13962=ORIENTED_EDGE('',*,*,#9571,.T.);
#13963=ORIENTED_EDGE('',*,*,#9684,.F.);
#13964=ORIENTED_EDGE('',*,*,#9599,.T.);
#13965=ORIENTED_EDGE('',*,*,#9410,.T.);
#13966=ORIENTED_EDGE('',*,*,#9569,.T.);
#13967=ORIENTED_EDGE('',*,*,#9407,.T.);
#13968=ORIENTED_EDGE('',*,*,#9606,.T.);
#13969=ORIENTED_EDGE('',*,*,#9685,.F.);
#13970=ORIENTED_EDGE('',*,*,#9566,.T.);
#13971=ORIENTED_EDGE('',*,*,#9686,.F.);
#13972=ORIENTED_EDGE('',*,*,#9604,.T.);
#13973=ORIENTED_EDGE('',*,*,#9404,.T.);
#13974=ORIENTED_EDGE('',*,*,#9564,.T.);
#13975=ORIENTED_EDGE('',*,*,#9401,.T.);
#13976=ORIENTED_EDGE('',*,*,#9611,.T.);
#13977=ORIENTED_EDGE('',*,*,#9687,.F.);
#13978=ORIENTED_EDGE('',*,*,#9561,.T.);
#13979=ORIENTED_EDGE('',*,*,#9688,.F.);
#13980=ORIENTED_EDGE('',*,*,#9609,.T.);
#13981=ORIENTED_EDGE('',*,*,#9398,.T.);
#13982=ORIENTED_EDGE('',*,*,#9559,.T.);
#13983=ORIENTED_EDGE('',*,*,#9395,.T.);
#13984=ORIENTED_EDGE('',*,*,#9616,.T.);
#13985=ORIENTED_EDGE('',*,*,#9689,.F.);
#13986=ORIENTED_EDGE('',*,*,#9556,.T.);
#13987=ORIENTED_EDGE('',*,*,#9690,.F.);
#13988=ORIENTED_EDGE('',*,*,#9614,.T.);
#13989=ORIENTED_EDGE('',*,*,#9392,.T.);
#13990=ORIENTED_EDGE('',*,*,#9554,.T.);
#13991=ORIENTED_EDGE('',*,*,#9389,.T.);
#13992=ORIENTED_EDGE('',*,*,#9621,.T.);
#13993=ORIENTED_EDGE('',*,*,#9691,.F.);
#13994=ORIENTED_EDGE('',*,*,#9551,.T.);
#13995=ORIENTED_EDGE('',*,*,#9692,.F.);
#13996=ORIENTED_EDGE('',*,*,#9619,.T.);
#13997=ORIENTED_EDGE('',*,*,#9386,.T.);
#13998=ORIENTED_EDGE('',*,*,#9549,.T.);
#13999=ORIENTED_EDGE('',*,*,#9383,.T.);
#14000=ORIENTED_EDGE('',*,*,#9626,.T.);
#14001=ORIENTED_EDGE('',*,*,#9693,.F.);
#14002=ORIENTED_EDGE('',*,*,#9546,.T.);
#14003=ORIENTED_EDGE('',*,*,#9694,.F.);
#14004=ORIENTED_EDGE('',*,*,#9624,.T.);
#14005=ORIENTED_EDGE('',*,*,#9380,.T.);
#14006=ORIENTED_EDGE('',*,*,#9541,.T.);
#14007=ORIENTED_EDGE('',*,*,#9695,.F.);
#14008=ORIENTED_EDGE('',*,*,#9544,.T.);
#14009=ORIENTED_EDGE('',*,*,#9377,.T.);
#14010=ORIENTED_EDGE('',*,*,#9539,.T.);
#14011=ORIENTED_EDGE('',*,*,#9374,.T.);
#14012=ORIENTED_EDGE('',*,*,#9636,.T.);
#14013=ORIENTED_EDGE('',*,*,#9696,.F.);
#14014=ORIENTED_EDGE('',*,*,#9536,.T.);
#14015=ORIENTED_EDGE('',*,*,#9697,.F.);
#14016=ORIENTED_EDGE('',*,*,#9634,.T.);
#14017=ORIENTED_EDGE('',*,*,#9371,.T.);
#14018=ORIENTED_EDGE('',*,*,#9534,.T.);
#14019=ORIENTED_EDGE('',*,*,#9368,.T.);
#14020=ORIENTED_EDGE('',*,*,#9641,.T.);
#14021=ORIENTED_EDGE('',*,*,#9698,.F.);
#14022=ORIENTED_EDGE('',*,*,#9531,.T.);
#14023=ORIENTED_EDGE('',*,*,#9699,.F.);
#14024=ORIENTED_EDGE('',*,*,#9639,.T.);
#14025=ORIENTED_EDGE('',*,*,#9365,.T.);
#14026=ORIENTED_EDGE('',*,*,#9529,.T.);
#14027=ORIENTED_EDGE('',*,*,#9362,.T.);
#14028=ORIENTED_EDGE('',*,*,#9646,.T.);
#14029=ORIENTED_EDGE('',*,*,#9700,.F.);
#14030=ORIENTED_EDGE('',*,*,#9526,.T.);
#14031=ORIENTED_EDGE('',*,*,#9701,.F.);
#14032=ORIENTED_EDGE('',*,*,#9644,.T.);
#14033=ORIENTED_EDGE('',*,*,#9359,.T.);
#14034=ORIENTED_EDGE('',*,*,#9524,.T.);
#14035=ORIENTED_EDGE('',*,*,#9356,.T.);
#14036=ORIENTED_EDGE('',*,*,#9651,.T.);
#14037=ORIENTED_EDGE('',*,*,#9702,.F.);
#14038=ORIENTED_EDGE('',*,*,#9521,.T.);
#14039=ORIENTED_EDGE('',*,*,#9703,.F.);
#14040=ORIENTED_EDGE('',*,*,#9649,.T.);
#14041=ORIENTED_EDGE('',*,*,#9353,.T.);
#14042=ORIENTED_EDGE('',*,*,#9519,.T.);
#14043=ORIENTED_EDGE('',*,*,#9350,.T.);
#14044=ORIENTED_EDGE('',*,*,#9656,.T.);
#14045=ORIENTED_EDGE('',*,*,#9704,.F.);
#14046=ORIENTED_EDGE('',*,*,#9516,.T.);
#14047=ORIENTED_EDGE('',*,*,#9705,.F.);
#14048=ORIENTED_EDGE('',*,*,#9654,.T.);
#14049=ORIENTED_EDGE('',*,*,#9347,.T.);
#14050=ORIENTED_EDGE('',*,*,#9514,.T.);
#14051=ORIENTED_EDGE('',*,*,#9344,.T.);
#14052=ORIENTED_EDGE('',*,*,#9661,.T.);
#14053=ORIENTED_EDGE('',*,*,#9706,.F.);
#14054=ORIENTED_EDGE('',*,*,#9511,.T.);
#14055=ORIENTED_EDGE('',*,*,#9707,.F.);
#14056=ORIENTED_EDGE('',*,*,#9659,.T.);
#14057=ORIENTED_EDGE('',*,*,#9341,.T.);
#14058=ORIENTED_EDGE('',*,*,#9509,.T.);
#14059=ORIENTED_EDGE('',*,*,#9338,.T.);
#14060=ORIENTED_EDGE('',*,*,#9666,.T.);
#14061=ORIENTED_EDGE('',*,*,#9708,.F.);
#14062=ORIENTED_EDGE('',*,*,#9506,.T.);
#14063=ORIENTED_EDGE('',*,*,#9709,.F.);
#14064=ORIENTED_EDGE('',*,*,#9664,.T.);
#14065=ORIENTED_EDGE('',*,*,#9335,.T.);
#14066=ORIENTED_EDGE('',*,*,#9504,.T.);
#14067=ORIENTED_EDGE('',*,*,#9332,.T.);
#14068=ORIENTED_EDGE('',*,*,#9671,.T.);
#14069=ORIENTED_EDGE('',*,*,#9710,.F.);
#14070=ORIENTED_EDGE('',*,*,#9501,.T.);
#14071=ORIENTED_EDGE('',*,*,#9711,.F.);
#14072=ORIENTED_EDGE('',*,*,#9669,.T.);
#14073=ORIENTED_EDGE('',*,*,#9329,.T.);
#14074=ORIENTED_EDGE('',*,*,#9499,.T.);
#14075=ORIENTED_EDGE('',*,*,#9434,.T.);
#14076=ORIENTED_EDGE('',*,*,#9676,.T.);
#14077=ORIENTED_EDGE('',*,*,#9712,.F.);
#14078=ORIENTED_EDGE('',*,*,#9713,.F.);
#14079=ORIENTED_EDGE('',*,*,#9318,.F.);
#14080=ORIENTED_EDGE('',*,*,#9179,.F.);
#14081=ORIENTED_EDGE('',*,*,#9319,.F.);
#14082=ORIENTED_EDGE('',*,*,#9714,.T.);
#14083=ORIENTED_EDGE('',*,*,#9713,.T.);
#14084=ORIENTED_EDGE('',*,*,#9714,.F.);
#14085=ORIENTED_EDGE('',*,*,#9715,.F.);
#14086=ORIENTED_EDGE('',*,*,#9716,.T.);
#14087=ORIENTED_EDGE('',*,*,#9537,.T.);
#14088=ORIENTED_EDGE('',*,*,#9696,.T.);
#14089=ORIENTED_EDGE('',*,*,#9635,.T.);
#14090=ORIENTED_EDGE('',*,*,#9632,.T.);
#14091=ORIENTED_EDGE('',*,*,#9697,.T.);
#14092=ORIENTED_EDGE('',*,*,#9535,.T.);
#14093=ORIENTED_EDGE('',*,*,#9532,.T.);
#14094=ORIENTED_EDGE('',*,*,#9698,.T.);
#14095=ORIENTED_EDGE('',*,*,#9640,.T.);
#14096=ORIENTED_EDGE('',*,*,#9637,.T.);
#14097=ORIENTED_EDGE('',*,*,#9699,.T.);
#14098=ORIENTED_EDGE('',*,*,#9530,.T.);
#14099=ORIENTED_EDGE('',*,*,#9527,.T.);
#14100=ORIENTED_EDGE('',*,*,#9700,.T.);
#14101=ORIENTED_EDGE('',*,*,#9645,.T.);
#14102=ORIENTED_EDGE('',*,*,#9642,.T.);
#14103=ORIENTED_EDGE('',*,*,#9701,.T.);
#14104=ORIENTED_EDGE('',*,*,#9525,.T.);
#14105=ORIENTED_EDGE('',*,*,#9522,.T.);
#14106=ORIENTED_EDGE('',*,*,#9702,.T.);
#14107=ORIENTED_EDGE('',*,*,#9650,.T.);
#14108=ORIENTED_EDGE('',*,*,#9647,.T.);
#14109=ORIENTED_EDGE('',*,*,#9703,.T.);
#14110=ORIENTED_EDGE('',*,*,#9520,.T.);
#14111=ORIENTED_EDGE('',*,*,#9517,.T.);
#14112=ORIENTED_EDGE('',*,*,#9704,.T.);
#14113=ORIENTED_EDGE('',*,*,#9655,.T.);
#14114=ORIENTED_EDGE('',*,*,#9652,.T.);
#14115=ORIENTED_EDGE('',*,*,#9705,.T.);
#14116=ORIENTED_EDGE('',*,*,#9515,.T.);
#14117=ORIENTED_EDGE('',*,*,#9512,.T.);
#14118=ORIENTED_EDGE('',*,*,#9706,.T.);
#14119=ORIENTED_EDGE('',*,*,#9660,.T.);
#14120=ORIENTED_EDGE('',*,*,#9657,.T.);
#14121=ORIENTED_EDGE('',*,*,#9707,.T.);
#14122=ORIENTED_EDGE('',*,*,#9510,.T.);
#14123=ORIENTED_EDGE('',*,*,#9507,.T.);
#14124=ORIENTED_EDGE('',*,*,#9708,.T.);
#14125=ORIENTED_EDGE('',*,*,#9665,.T.);
#14126=ORIENTED_EDGE('',*,*,#9662,.T.);
#14127=ORIENTED_EDGE('',*,*,#9709,.T.);
#14128=ORIENTED_EDGE('',*,*,#9505,.T.);
#14129=ORIENTED_EDGE('',*,*,#9502,.T.);
#14130=ORIENTED_EDGE('',*,*,#9710,.T.);
#14131=ORIENTED_EDGE('',*,*,#9670,.T.);
#14132=ORIENTED_EDGE('',*,*,#9667,.T.);
#14133=ORIENTED_EDGE('',*,*,#9711,.T.);
#14134=ORIENTED_EDGE('',*,*,#9500,.T.);
#14135=ORIENTED_EDGE('',*,*,#9497,.T.);
#14136=ORIENTED_EDGE('',*,*,#9712,.T.);
#14137=ORIENTED_EDGE('',*,*,#9675,.T.);
#14138=ORIENTED_EDGE('',*,*,#9672,.T.);
#14139=ORIENTED_EDGE('',*,*,#9677,.T.);
#14140=ORIENTED_EDGE('',*,*,#9630,.T.);
#14141=ORIENTED_EDGE('',*,*,#9627,.T.);
#14142=ORIENTED_EDGE('',*,*,#9678,.T.);
#14143=ORIENTED_EDGE('',*,*,#9585,.T.);
#14144=ORIENTED_EDGE('',*,*,#9582,.T.);
#14145=ORIENTED_EDGE('',*,*,#9679,.T.);
#14146=ORIENTED_EDGE('',*,*,#9590,.T.);
#14147=ORIENTED_EDGE('',*,*,#9587,.T.);
#14148=ORIENTED_EDGE('',*,*,#9680,.T.);
#14149=ORIENTED_EDGE('',*,*,#9580,.T.);
#14150=ORIENTED_EDGE('',*,*,#9577,.T.);
#14151=ORIENTED_EDGE('',*,*,#9681,.T.);
#14152=ORIENTED_EDGE('',*,*,#9595,.T.);
#14153=ORIENTED_EDGE('',*,*,#9592,.T.);
#14154=ORIENTED_EDGE('',*,*,#9682,.T.);
#14155=ORIENTED_EDGE('',*,*,#9575,.T.);
#14156=ORIENTED_EDGE('',*,*,#9572,.T.);
#14157=ORIENTED_EDGE('',*,*,#9683,.T.);
#14158=ORIENTED_EDGE('',*,*,#9600,.T.);
#14159=ORIENTED_EDGE('',*,*,#9597,.T.);
#14160=ORIENTED_EDGE('',*,*,#9684,.T.);
#14161=ORIENTED_EDGE('',*,*,#9570,.T.);
#14162=ORIENTED_EDGE('',*,*,#9567,.T.);
#14163=ORIENTED_EDGE('',*,*,#9685,.T.);
#14164=ORIENTED_EDGE('',*,*,#9605,.T.);
#14165=ORIENTED_EDGE('',*,*,#9602,.T.);
#14166=ORIENTED_EDGE('',*,*,#9686,.T.);
#14167=ORIENTED_EDGE('',*,*,#9565,.T.);
#14168=ORIENTED_EDGE('',*,*,#9562,.T.);
#14169=ORIENTED_EDGE('',*,*,#9687,.T.);
#14170=ORIENTED_EDGE('',*,*,#9610,.T.);
#14171=ORIENTED_EDGE('',*,*,#9607,.T.);
#14172=ORIENTED_EDGE('',*,*,#9688,.T.);
#14173=ORIENTED_EDGE('',*,*,#9560,.T.);
#14174=ORIENTED_EDGE('',*,*,#9557,.T.);
#14175=ORIENTED_EDGE('',*,*,#9689,.T.);
#14176=ORIENTED_EDGE('',*,*,#9615,.T.);
#14177=ORIENTED_EDGE('',*,*,#9612,.T.);
#14178=ORIENTED_EDGE('',*,*,#9690,.T.);
#14179=ORIENTED_EDGE('',*,*,#9555,.T.);
#14180=ORIENTED_EDGE('',*,*,#9552,.T.);
#14181=ORIENTED_EDGE('',*,*,#9691,.T.);
#14182=ORIENTED_EDGE('',*,*,#9620,.T.);
#14183=ORIENTED_EDGE('',*,*,#9617,.T.);
#14184=ORIENTED_EDGE('',*,*,#9692,.T.);
#14185=ORIENTED_EDGE('',*,*,#9550,.T.);
#14186=ORIENTED_EDGE('',*,*,#9547,.T.);
#14187=ORIENTED_EDGE('',*,*,#9693,.T.);
#14188=ORIENTED_EDGE('',*,*,#9625,.T.);
#14189=ORIENTED_EDGE('',*,*,#9622,.T.);
#14190=ORIENTED_EDGE('',*,*,#9694,.T.);
#14191=ORIENTED_EDGE('',*,*,#9545,.T.);
#14192=ORIENTED_EDGE('',*,*,#9542,.T.);
#14193=ORIENTED_EDGE('',*,*,#9695,.T.);
#14194=ORIENTED_EDGE('',*,*,#9540,.T.);
#14195=ORIENTED_EDGE('',*,*,#9716,.F.);
#14196=ORIENTED_EDGE('',*,*,#9715,.T.);
#14197=ORIENTED_EDGE('',*,*,#9483,.T.);
#14198=ORIENTED_EDGE('',*,*,#9494,.T.);
#14199=ORIENTED_EDGE('',*,*,#9496,.T.);
#14200=ORIENTED_EDGE('',*,*,#9478,.T.);
#14201=ORIENTED_EDGE('',*,*,#9468,.T.);
#14202=ORIENTED_EDGE('',*,*,#9473,.T.);
#14203=ORIENTED_EDGE('',*,*,#9717,.F.);
#14204=ORIENTED_EDGE('',*,*,#9718,.T.);
#14205=ORIENTED_EDGE('',*,*,#9719,.T.);
#14206=ORIENTED_EDGE('',*,*,#9720,.T.);
#14207=ORIENTED_EDGE('',*,*,#9721,.F.);
#14208=ORIENTED_EDGE('',*,*,#9722,.T.);
#14209=ORIENTED_EDGE('',*,*,#9717,.T.);
#14210=ORIENTED_EDGE('',*,*,#9723,.T.);
#14211=ORIENTED_EDGE('',*,*,#9724,.F.);
#14212=ORIENTED_EDGE('',*,*,#9725,.T.);
#14213=ORIENTED_EDGE('',*,*,#9721,.T.);
#14214=ORIENTED_EDGE('',*,*,#9726,.T.);
#14215=ORIENTED_EDGE('',*,*,#9727,.F.);
#14216=ORIENTED_EDGE('',*,*,#9728,.T.);
#14217=ORIENTED_EDGE('',*,*,#9724,.T.);
#14218=ORIENTED_EDGE('',*,*,#9729,.T.);
#14219=ORIENTED_EDGE('',*,*,#9730,.F.);
#14220=ORIENTED_EDGE('',*,*,#9731,.T.);
#14221=ORIENTED_EDGE('',*,*,#9727,.T.);
#14222=ORIENTED_EDGE('',*,*,#9732,.T.);
#14223=ORIENTED_EDGE('',*,*,#9733,.F.);
#14224=ORIENTED_EDGE('',*,*,#9734,.T.);
#14225=ORIENTED_EDGE('',*,*,#9730,.T.);
#14226=ORIENTED_EDGE('',*,*,#9735,.T.);
#14227=ORIENTED_EDGE('',*,*,#9736,.F.);
#14228=ORIENTED_EDGE('',*,*,#9737,.T.);
#14229=ORIENTED_EDGE('',*,*,#9733,.T.);
#14230=ORIENTED_EDGE('',*,*,#9738,.T.);
#14231=ORIENTED_EDGE('',*,*,#9739,.F.);
#14232=ORIENTED_EDGE('',*,*,#9740,.T.);
#14233=ORIENTED_EDGE('',*,*,#9736,.T.);
#14234=ORIENTED_EDGE('',*,*,#9741,.T.);
#14235=ORIENTED_EDGE('',*,*,#9742,.F.);
#14236=ORIENTED_EDGE('',*,*,#9743,.T.);
#14237=ORIENTED_EDGE('',*,*,#9739,.T.);
#14238=ORIENTED_EDGE('',*,*,#9744,.T.);
#14239=ORIENTED_EDGE('',*,*,#9745,.F.);
#14240=ORIENTED_EDGE('',*,*,#9746,.T.);
#14241=ORIENTED_EDGE('',*,*,#9742,.T.);
#14242=ORIENTED_EDGE('',*,*,#9747,.T.);
#14243=ORIENTED_EDGE('',*,*,#9748,.F.);
#14244=ORIENTED_EDGE('',*,*,#9749,.T.);
#14245=ORIENTED_EDGE('',*,*,#9745,.T.);
#14246=ORIENTED_EDGE('',*,*,#9750,.T.);
#14247=ORIENTED_EDGE('',*,*,#9751,.F.);
#14248=ORIENTED_EDGE('',*,*,#9752,.T.);
#14249=ORIENTED_EDGE('',*,*,#9753,.F.);
#14250=ORIENTED_EDGE('',*,*,#9754,.F.);
#14251=ORIENTED_EDGE('',*,*,#9755,.F.);
#14252=ORIENTED_EDGE('',*,*,#9756,.T.);
#14253=ORIENTED_EDGE('',*,*,#9751,.T.);
#14254=ORIENTED_EDGE('',*,*,#9757,.F.);
#14255=ORIENTED_EDGE('',*,*,#9758,.F.);
#14256=ORIENTED_EDGE('',*,*,#9759,.T.);
#14257=ORIENTED_EDGE('',*,*,#9755,.T.);
#14258=ORIENTED_EDGE('',*,*,#9760,.F.);
#14259=ORIENTED_EDGE('',*,*,#9761,.F.);
#14260=ORIENTED_EDGE('',*,*,#9762,.T.);
#14261=ORIENTED_EDGE('',*,*,#9758,.T.);
#14262=ORIENTED_EDGE('',*,*,#9763,.F.);
#14263=ORIENTED_EDGE('',*,*,#9764,.F.);
#14264=ORIENTED_EDGE('',*,*,#9765,.T.);
#14265=ORIENTED_EDGE('',*,*,#9761,.T.);
#14266=ORIENTED_EDGE('',*,*,#9766,.F.);
#14267=ORIENTED_EDGE('',*,*,#9767,.F.);
#14268=ORIENTED_EDGE('',*,*,#9768,.T.);
#14269=ORIENTED_EDGE('',*,*,#9764,.T.);
#14270=ORIENTED_EDGE('',*,*,#9769,.F.);
#14271=ORIENTED_EDGE('',*,*,#9770,.F.);
#14272=ORIENTED_EDGE('',*,*,#9771,.T.);
#14273=ORIENTED_EDGE('',*,*,#9767,.T.);
#14274=ORIENTED_EDGE('',*,*,#9772,.F.);
#14275=ORIENTED_EDGE('',*,*,#9773,.F.);
#14276=ORIENTED_EDGE('',*,*,#9774,.T.);
#14277=ORIENTED_EDGE('',*,*,#9770,.T.);
#14278=ORIENTED_EDGE('',*,*,#9775,.F.);
#14279=ORIENTED_EDGE('',*,*,#9776,.F.);
#14280=ORIENTED_EDGE('',*,*,#9777,.T.);
#14281=ORIENTED_EDGE('',*,*,#9773,.T.);
#14282=ORIENTED_EDGE('',*,*,#9778,.F.);
#14283=ORIENTED_EDGE('',*,*,#9779,.F.);
#14284=ORIENTED_EDGE('',*,*,#9780,.T.);
#14285=ORIENTED_EDGE('',*,*,#9776,.T.);
#14286=ORIENTED_EDGE('',*,*,#9781,.F.);
#14287=ORIENTED_EDGE('',*,*,#9782,.F.);
#14288=ORIENTED_EDGE('',*,*,#9783,.T.);
#14289=ORIENTED_EDGE('',*,*,#9779,.T.);
#14290=ORIENTED_EDGE('',*,*,#9784,.F.);
#14291=ORIENTED_EDGE('',*,*,#9785,.F.);
#14292=ORIENTED_EDGE('',*,*,#9786,.F.);
#14293=ORIENTED_EDGE('',*,*,#9750,.F.);
#14294=ORIENTED_EDGE('',*,*,#9747,.F.);
#14295=ORIENTED_EDGE('',*,*,#9744,.F.);
#14296=ORIENTED_EDGE('',*,*,#9741,.F.);
#14297=ORIENTED_EDGE('',*,*,#9738,.F.);
#14298=ORIENTED_EDGE('',*,*,#9735,.F.);
#14299=ORIENTED_EDGE('',*,*,#9732,.F.);
#14300=ORIENTED_EDGE('',*,*,#9729,.F.);
#14301=ORIENTED_EDGE('',*,*,#9726,.F.);
#14302=ORIENTED_EDGE('',*,*,#9723,.F.);
#14303=ORIENTED_EDGE('',*,*,#9720,.F.);
#14304=ORIENTED_EDGE('',*,*,#9787,.F.);
#14305=ORIENTED_EDGE('',*,*,#9788,.T.);
#14306=ORIENTED_EDGE('',*,*,#9784,.T.);
#14307=ORIENTED_EDGE('',*,*,#9781,.T.);
#14308=ORIENTED_EDGE('',*,*,#9778,.T.);
#14309=ORIENTED_EDGE('',*,*,#9775,.T.);
#14310=ORIENTED_EDGE('',*,*,#9772,.T.);
#14311=ORIENTED_EDGE('',*,*,#9769,.T.);
#14312=ORIENTED_EDGE('',*,*,#9766,.T.);
#14313=ORIENTED_EDGE('',*,*,#9763,.T.);
#14314=ORIENTED_EDGE('',*,*,#9760,.T.);
#14315=ORIENTED_EDGE('',*,*,#9757,.T.);
#14316=ORIENTED_EDGE('',*,*,#9754,.T.);
#14317=ORIENTED_EDGE('',*,*,#9789,.T.);
#14318=ORIENTED_EDGE('',*,*,#9790,.T.);
#14319=ORIENTED_EDGE('',*,*,#9791,.T.);
#14320=ORIENTED_EDGE('',*,*,#9792,.T.);
#14321=ORIENTED_EDGE('',*,*,#9787,.T.);
#14322=ORIENTED_EDGE('',*,*,#9782,.T.);
#14323=ORIENTED_EDGE('',*,*,#9788,.F.);
#14324=ORIENTED_EDGE('',*,*,#9792,.F.);
#14325=ORIENTED_EDGE('',*,*,#9793,.T.);
#14326=ORIENTED_EDGE('',*,*,#9794,.F.);
#14327=ORIENTED_EDGE('',*,*,#9752,.F.);
#14328=ORIENTED_EDGE('',*,*,#9756,.F.);
#14329=ORIENTED_EDGE('',*,*,#9759,.F.);
#14330=ORIENTED_EDGE('',*,*,#9762,.F.);
#14331=ORIENTED_EDGE('',*,*,#9765,.F.);
#14332=ORIENTED_EDGE('',*,*,#9768,.F.);
#14333=ORIENTED_EDGE('',*,*,#9771,.F.);
#14334=ORIENTED_EDGE('',*,*,#9774,.F.);
#14335=ORIENTED_EDGE('',*,*,#9777,.F.);
#14336=ORIENTED_EDGE('',*,*,#9780,.F.);
#14337=ORIENTED_EDGE('',*,*,#9783,.F.);
#14338=ORIENTED_EDGE('',*,*,#9793,.F.);
#14339=ORIENTED_EDGE('',*,*,#9791,.F.);
#14340=ORIENTED_EDGE('',*,*,#9718,.F.);
#14341=ORIENTED_EDGE('',*,*,#9722,.F.);
#14342=ORIENTED_EDGE('',*,*,#9725,.F.);
#14343=ORIENTED_EDGE('',*,*,#9728,.F.);
#14344=ORIENTED_EDGE('',*,*,#9731,.F.);
#14345=ORIENTED_EDGE('',*,*,#9734,.F.);
#14346=ORIENTED_EDGE('',*,*,#9737,.F.);
#14347=ORIENTED_EDGE('',*,*,#9740,.F.);
#14348=ORIENTED_EDGE('',*,*,#9743,.F.);
#14349=ORIENTED_EDGE('',*,*,#9746,.F.);
#14350=ORIENTED_EDGE('',*,*,#9749,.F.);
#14351=ORIENTED_EDGE('',*,*,#9795,.F.);
#14352=ORIENTED_EDGE('',*,*,#9796,.F.);
#14353=ORIENTED_EDGE('',*,*,#9797,.T.);
#14354=ORIENTED_EDGE('',*,*,#9798,.F.);
#14355=ORIENTED_EDGE('',*,*,#9799,.F.);
#14356=ORIENTED_EDGE('',*,*,#9800,.F.);
#14357=ORIENTED_EDGE('',*,*,#9801,.F.);
#14358=ORIENTED_EDGE('',*,*,#9802,.F.);
#14359=ORIENTED_EDGE('',*,*,#9797,.F.);
#14360=ORIENTED_EDGE('',*,*,#9803,.F.);
#14361=ORIENTED_EDGE('',*,*,#9804,.T.);
#14362=ORIENTED_EDGE('',*,*,#9805,.F.);
#14363=ORIENTED_EDGE('',*,*,#9806,.F.);
#14364=ORIENTED_EDGE('',*,*,#9807,.F.);
#14365=ORIENTED_EDGE('',*,*,#9808,.F.);
#14366=ORIENTED_EDGE('',*,*,#9809,.F.);
#14367=ORIENTED_EDGE('',*,*,#9804,.F.);
#14368=ORIENTED_EDGE('',*,*,#9810,.F.);
#14369=ORIENTED_EDGE('',*,*,#9811,.T.);
#14370=ORIENTED_EDGE('',*,*,#9812,.F.);
#14371=ORIENTED_EDGE('',*,*,#9813,.F.);
#14372=ORIENTED_EDGE('',*,*,#9814,.F.);
#14373=ORIENTED_EDGE('',*,*,#9815,.F.);
#14374=ORIENTED_EDGE('',*,*,#9816,.F.);
#14375=ORIENTED_EDGE('',*,*,#9811,.F.);
#14376=ORIENTED_EDGE('',*,*,#9817,.F.);
#14377=ORIENTED_EDGE('',*,*,#9818,.T.);
#14378=ORIENTED_EDGE('',*,*,#9819,.F.);
#14379=ORIENTED_EDGE('',*,*,#9820,.F.);
#14380=ORIENTED_EDGE('',*,*,#9821,.F.);
#14381=ORIENTED_EDGE('',*,*,#9822,.F.);
#14382=ORIENTED_EDGE('',*,*,#9823,.F.);
#14383=ORIENTED_EDGE('',*,*,#9818,.F.);
#14384=ORIENTED_EDGE('',*,*,#9824,.F.);
#14385=ORIENTED_EDGE('',*,*,#9825,.T.);
#14386=ORIENTED_EDGE('',*,*,#9826,.F.);
#14387=ORIENTED_EDGE('',*,*,#9827,.F.);
#14388=ORIENTED_EDGE('',*,*,#9828,.F.);
#14389=ORIENTED_EDGE('',*,*,#9829,.F.);
#14390=ORIENTED_EDGE('',*,*,#9830,.F.);
#14391=ORIENTED_EDGE('',*,*,#9825,.F.);
#14392=ORIENTED_EDGE('',*,*,#9831,.F.);
#14393=ORIENTED_EDGE('',*,*,#9832,.T.);
#14394=ORIENTED_EDGE('',*,*,#9833,.F.);
#14395=ORIENTED_EDGE('',*,*,#9834,.F.);
#14396=ORIENTED_EDGE('',*,*,#9835,.F.);
#14397=ORIENTED_EDGE('',*,*,#9836,.F.);
#14398=ORIENTED_EDGE('',*,*,#9837,.F.);
#14399=ORIENTED_EDGE('',*,*,#9832,.F.);
#14400=ORIENTED_EDGE('',*,*,#9838,.F.);
#14401=ORIENTED_EDGE('',*,*,#9839,.T.);
#14402=ORIENTED_EDGE('',*,*,#9840,.F.);
#14403=ORIENTED_EDGE('',*,*,#9841,.F.);
#14404=ORIENTED_EDGE('',*,*,#9842,.F.);
#14405=ORIENTED_EDGE('',*,*,#9843,.F.);
#14406=ORIENTED_EDGE('',*,*,#9844,.F.);
#14407=ORIENTED_EDGE('',*,*,#9839,.F.);
#14408=ORIENTED_EDGE('',*,*,#9845,.F.);
#14409=ORIENTED_EDGE('',*,*,#9846,.T.);
#14410=ORIENTED_EDGE('',*,*,#9847,.F.);
#14411=ORIENTED_EDGE('',*,*,#9848,.F.);
#14412=ORIENTED_EDGE('',*,*,#9849,.F.);
#14413=ORIENTED_EDGE('',*,*,#9850,.F.);
#14414=ORIENTED_EDGE('',*,*,#9851,.F.);
#14415=ORIENTED_EDGE('',*,*,#9846,.F.);
#14416=ORIENTED_EDGE('',*,*,#9852,.F.);
#14417=ORIENTED_EDGE('',*,*,#9853,.T.);
#14418=ORIENTED_EDGE('',*,*,#9854,.F.);
#14419=ORIENTED_EDGE('',*,*,#9855,.F.);
#14420=ORIENTED_EDGE('',*,*,#9856,.F.);
#14421=ORIENTED_EDGE('',*,*,#9857,.F.);
#14422=ORIENTED_EDGE('',*,*,#9858,.F.);
#14423=ORIENTED_EDGE('',*,*,#9853,.F.);
#14424=ORIENTED_EDGE('',*,*,#9859,.F.);
#14425=ORIENTED_EDGE('',*,*,#9860,.T.);
#14426=ORIENTED_EDGE('',*,*,#9861,.F.);
#14427=ORIENTED_EDGE('',*,*,#9862,.F.);
#14428=ORIENTED_EDGE('',*,*,#9863,.F.);
#14429=ORIENTED_EDGE('',*,*,#9864,.F.);
#14430=ORIENTED_EDGE('',*,*,#9865,.F.);
#14431=ORIENTED_EDGE('',*,*,#9860,.F.);
#14432=ORIENTED_EDGE('',*,*,#9866,.F.);
#14433=ORIENTED_EDGE('',*,*,#9867,.T.);
#14434=ORIENTED_EDGE('',*,*,#9868,.F.);
#14435=ORIENTED_EDGE('',*,*,#9869,.F.);
#14436=ORIENTED_EDGE('',*,*,#9870,.F.);
#14437=ORIENTED_EDGE('',*,*,#9871,.F.);
#14438=ORIENTED_EDGE('',*,*,#9872,.F.);
#14439=ORIENTED_EDGE('',*,*,#9867,.F.);
#14440=ORIENTED_EDGE('',*,*,#9873,.F.);
#14441=ORIENTED_EDGE('',*,*,#9874,.T.);
#14442=ORIENTED_EDGE('',*,*,#9875,.F.);
#14443=ORIENTED_EDGE('',*,*,#9876,.F.);
#14444=ORIENTED_EDGE('',*,*,#9877,.F.);
#14445=ORIENTED_EDGE('',*,*,#9878,.F.);
#14446=ORIENTED_EDGE('',*,*,#9879,.F.);
#14447=ORIENTED_EDGE('',*,*,#9874,.F.);
#14448=ORIENTED_EDGE('',*,*,#9880,.F.);
#14449=ORIENTED_EDGE('',*,*,#9881,.T.);
#14450=ORIENTED_EDGE('',*,*,#9882,.F.);
#14451=ORIENTED_EDGE('',*,*,#9883,.F.);
#14452=ORIENTED_EDGE('',*,*,#9884,.F.);
#14453=ORIENTED_EDGE('',*,*,#9885,.F.);
#14454=ORIENTED_EDGE('',*,*,#9886,.F.);
#14455=ORIENTED_EDGE('',*,*,#9881,.F.);
#14456=ORIENTED_EDGE('',*,*,#9887,.F.);
#14457=ORIENTED_EDGE('',*,*,#9888,.T.);
#14458=ORIENTED_EDGE('',*,*,#9889,.F.);
#14459=ORIENTED_EDGE('',*,*,#9890,.F.);
#14460=ORIENTED_EDGE('',*,*,#9891,.F.);
#14461=ORIENTED_EDGE('',*,*,#9892,.F.);
#14462=ORIENTED_EDGE('',*,*,#9893,.F.);
#14463=ORIENTED_EDGE('',*,*,#9888,.F.);
#14464=ORIENTED_EDGE('',*,*,#9894,.F.);
#14465=ORIENTED_EDGE('',*,*,#9895,.T.);
#14466=ORIENTED_EDGE('',*,*,#9896,.F.);
#14467=ORIENTED_EDGE('',*,*,#9897,.F.);
#14468=ORIENTED_EDGE('',*,*,#9898,.F.);
#14469=ORIENTED_EDGE('',*,*,#9899,.F.);
#14470=ORIENTED_EDGE('',*,*,#9900,.F.);
#14471=ORIENTED_EDGE('',*,*,#9895,.F.);
#14472=ORIENTED_EDGE('',*,*,#9901,.F.);
#14473=ORIENTED_EDGE('',*,*,#9902,.T.);
#14474=ORIENTED_EDGE('',*,*,#9903,.F.);
#14475=ORIENTED_EDGE('',*,*,#9904,.F.);
#14476=ORIENTED_EDGE('',*,*,#9905,.F.);
#14477=ORIENTED_EDGE('',*,*,#9906,.F.);
#14478=ORIENTED_EDGE('',*,*,#9907,.F.);
#14479=ORIENTED_EDGE('',*,*,#9902,.F.);
#14480=ORIENTED_EDGE('',*,*,#9908,.F.);
#14481=ORIENTED_EDGE('',*,*,#9909,.T.);
#14482=ORIENTED_EDGE('',*,*,#9910,.F.);
#14483=ORIENTED_EDGE('',*,*,#9911,.F.);
#14484=ORIENTED_EDGE('',*,*,#9912,.F.);
#14485=ORIENTED_EDGE('',*,*,#9913,.F.);
#14486=ORIENTED_EDGE('',*,*,#9914,.F.);
#14487=ORIENTED_EDGE('',*,*,#9909,.F.);
#14488=ORIENTED_EDGE('',*,*,#9915,.F.);
#14489=ORIENTED_EDGE('',*,*,#9916,.T.);
#14490=ORIENTED_EDGE('',*,*,#9917,.F.);
#14491=ORIENTED_EDGE('',*,*,#9918,.F.);
#14492=ORIENTED_EDGE('',*,*,#9919,.F.);
#14493=ORIENTED_EDGE('',*,*,#9920,.F.);
#14494=ORIENTED_EDGE('',*,*,#9921,.F.);
#14495=ORIENTED_EDGE('',*,*,#9916,.F.);
#14496=ORIENTED_EDGE('',*,*,#9922,.F.);
#14497=ORIENTED_EDGE('',*,*,#9923,.T.);
#14498=ORIENTED_EDGE('',*,*,#9924,.F.);
#14499=ORIENTED_EDGE('',*,*,#9925,.F.);
#14500=ORIENTED_EDGE('',*,*,#9926,.F.);
#14501=ORIENTED_EDGE('',*,*,#9927,.F.);
#14502=ORIENTED_EDGE('',*,*,#9928,.F.);
#14503=ORIENTED_EDGE('',*,*,#9923,.F.);
#14504=ORIENTED_EDGE('',*,*,#9929,.F.);
#14505=ORIENTED_EDGE('',*,*,#9930,.T.);
#14506=ORIENTED_EDGE('',*,*,#9931,.F.);
#14507=ORIENTED_EDGE('',*,*,#9932,.F.);
#14508=ORIENTED_EDGE('',*,*,#9933,.F.);
#14509=ORIENTED_EDGE('',*,*,#9934,.F.);
#14510=ORIENTED_EDGE('',*,*,#9935,.F.);
#14511=ORIENTED_EDGE('',*,*,#9930,.F.);
#14512=ORIENTED_EDGE('',*,*,#9936,.F.);
#14513=ORIENTED_EDGE('',*,*,#9937,.T.);
#14514=ORIENTED_EDGE('',*,*,#9938,.F.);
#14515=ORIENTED_EDGE('',*,*,#9939,.F.);
#14516=ORIENTED_EDGE('',*,*,#9940,.F.);
#14517=ORIENTED_EDGE('',*,*,#9941,.F.);
#14518=ORIENTED_EDGE('',*,*,#9942,.F.);
#14519=ORIENTED_EDGE('',*,*,#9937,.F.);
#14520=ORIENTED_EDGE('',*,*,#9943,.F.);
#14521=ORIENTED_EDGE('',*,*,#9944,.T.);
#14522=ORIENTED_EDGE('',*,*,#9945,.F.);
#14523=ORIENTED_EDGE('',*,*,#9946,.F.);
#14524=ORIENTED_EDGE('',*,*,#9947,.F.);
#14525=ORIENTED_EDGE('',*,*,#9948,.F.);
#14526=ORIENTED_EDGE('',*,*,#9949,.F.);
#14527=ORIENTED_EDGE('',*,*,#9944,.F.);
#14528=ORIENTED_EDGE('',*,*,#9950,.F.);
#14529=ORIENTED_EDGE('',*,*,#9951,.T.);
#14530=ORIENTED_EDGE('',*,*,#9952,.F.);
#14531=ORIENTED_EDGE('',*,*,#9953,.F.);
#14532=ORIENTED_EDGE('',*,*,#9954,.F.);
#14533=ORIENTED_EDGE('',*,*,#9955,.F.);
#14534=ORIENTED_EDGE('',*,*,#9956,.F.);
#14535=ORIENTED_EDGE('',*,*,#9951,.F.);
#14536=ORIENTED_EDGE('',*,*,#9957,.F.);
#14537=ORIENTED_EDGE('',*,*,#9958,.T.);
#14538=ORIENTED_EDGE('',*,*,#9959,.F.);
#14539=ORIENTED_EDGE('',*,*,#9960,.F.);
#14540=ORIENTED_EDGE('',*,*,#9961,.F.);
#14541=ORIENTED_EDGE('',*,*,#9962,.F.);
#14542=ORIENTED_EDGE('',*,*,#9963,.F.);
#14543=ORIENTED_EDGE('',*,*,#9958,.F.);
#14544=ORIENTED_EDGE('',*,*,#9920,.T.);
#14545=ORIENTED_EDGE('',*,*,#9964,.F.);
#14546=ORIENTED_EDGE('',*,*,#9960,.T.);
#14547=ORIENTED_EDGE('',*,*,#9965,.T.);
#14548=ORIENTED_EDGE('',*,*,#9878,.T.);
#14549=ORIENTED_EDGE('',*,*,#9966,.F.);
#14550=ORIENTED_EDGE('',*,*,#9918,.T.);
#14551=ORIENTED_EDGE('',*,*,#9967,.T.);
#14552=ORIENTED_EDGE('',*,*,#9876,.T.);
#14553=ORIENTED_EDGE('',*,*,#9968,.T.);
#14554=ORIENTED_EDGE('',*,*,#9885,.T.);
#14555=ORIENTED_EDGE('',*,*,#9969,.F.);
#14556=ORIENTED_EDGE('',*,*,#9871,.T.);
#14557=ORIENTED_EDGE('',*,*,#9970,.F.);
#14558=ORIENTED_EDGE('',*,*,#9883,.T.);
#14559=ORIENTED_EDGE('',*,*,#9971,.T.);
#14560=ORIENTED_EDGE('',*,*,#9869,.T.);
#14561=ORIENTED_EDGE('',*,*,#9972,.T.);
#14562=ORIENTED_EDGE('',*,*,#9892,.T.);
#14563=ORIENTED_EDGE('',*,*,#9973,.F.);
#14564=ORIENTED_EDGE('',*,*,#9864,.T.);
#14565=ORIENTED_EDGE('',*,*,#9974,.F.);
#14566=ORIENTED_EDGE('',*,*,#9890,.T.);
#14567=ORIENTED_EDGE('',*,*,#9975,.T.);
#14568=ORIENTED_EDGE('',*,*,#9862,.T.);
#14569=ORIENTED_EDGE('',*,*,#9976,.T.);
#14570=ORIENTED_EDGE('',*,*,#9899,.T.);
#14571=ORIENTED_EDGE('',*,*,#9977,.F.);
#14572=ORIENTED_EDGE('',*,*,#9857,.T.);
#14573=ORIENTED_EDGE('',*,*,#9978,.F.);
#14574=ORIENTED_EDGE('',*,*,#9897,.T.);
#14575=ORIENTED_EDGE('',*,*,#9979,.T.);
#14576=ORIENTED_EDGE('',*,*,#9855,.T.);
#14577=ORIENTED_EDGE('',*,*,#9980,.T.);
#14578=ORIENTED_EDGE('',*,*,#9906,.T.);
#14579=ORIENTED_EDGE('',*,*,#9981,.F.);
#14580=ORIENTED_EDGE('',*,*,#9850,.T.);
#14581=ORIENTED_EDGE('',*,*,#9982,.F.);
#14582=ORIENTED_EDGE('',*,*,#9904,.T.);
#14583=ORIENTED_EDGE('',*,*,#9983,.T.);
#14584=ORIENTED_EDGE('',*,*,#9848,.T.);
#14585=ORIENTED_EDGE('',*,*,#9984,.T.);
#14586=ORIENTED_EDGE('',*,*,#9913,.T.);
#14587=ORIENTED_EDGE('',*,*,#9985,.F.);
#14588=ORIENTED_EDGE('',*,*,#9843,.T.);
#14589=ORIENTED_EDGE('',*,*,#9986,.F.);
#14590=ORIENTED_EDGE('',*,*,#9911,.T.);
#14591=ORIENTED_EDGE('',*,*,#9987,.T.);
#14592=ORIENTED_EDGE('',*,*,#9836,.T.);
#14593=ORIENTED_EDGE('',*,*,#9988,.F.);
#14594=ORIENTED_EDGE('',*,*,#9841,.T.);
#14595=ORIENTED_EDGE('',*,*,#9989,.T.);
#14596=ORIENTED_EDGE('',*,*,#9834,.T.);
#14597=ORIENTED_EDGE('',*,*,#9990,.T.);
#14598=ORIENTED_EDGE('',*,*,#9927,.T.);
#14599=ORIENTED_EDGE('',*,*,#9991,.F.);
#14600=ORIENTED_EDGE('',*,*,#9829,.T.);
#14601=ORIENTED_EDGE('',*,*,#9992,.F.);
#14602=ORIENTED_EDGE('',*,*,#9925,.T.);
#14603=ORIENTED_EDGE('',*,*,#9993,.T.);
#14604=ORIENTED_EDGE('',*,*,#9827,.T.);
#14605=ORIENTED_EDGE('',*,*,#9994,.T.);
#14606=ORIENTED_EDGE('',*,*,#9934,.T.);
#14607=ORIENTED_EDGE('',*,*,#9995,.F.);
#14608=ORIENTED_EDGE('',*,*,#9822,.T.);
#14609=ORIENTED_EDGE('',*,*,#9996,.F.);
#14610=ORIENTED_EDGE('',*,*,#9932,.T.);
#14611=ORIENTED_EDGE('',*,*,#9997,.T.);
#14612=ORIENTED_EDGE('',*,*,#9820,.T.);
#14613=ORIENTED_EDGE('',*,*,#9998,.T.);
#14614=ORIENTED_EDGE('',*,*,#9941,.T.);
#14615=ORIENTED_EDGE('',*,*,#9999,.F.);
#14616=ORIENTED_EDGE('',*,*,#9815,.T.);
#14617=ORIENTED_EDGE('',*,*,#10000,.F.);
#14618=ORIENTED_EDGE('',*,*,#9939,.T.);
#14619=ORIENTED_EDGE('',*,*,#10001,.T.);
#14620=ORIENTED_EDGE('',*,*,#9813,.T.);
#14621=ORIENTED_EDGE('',*,*,#10002,.T.);
#14622=ORIENTED_EDGE('',*,*,#9948,.T.);
#14623=ORIENTED_EDGE('',*,*,#10003,.F.);
#14624=ORIENTED_EDGE('',*,*,#9808,.T.);
#14625=ORIENTED_EDGE('',*,*,#10004,.F.);
#14626=ORIENTED_EDGE('',*,*,#9946,.T.);
#14627=ORIENTED_EDGE('',*,*,#10005,.T.);
#14628=ORIENTED_EDGE('',*,*,#9806,.T.);
#14629=ORIENTED_EDGE('',*,*,#10006,.T.);
#14630=ORIENTED_EDGE('',*,*,#9955,.T.);
#14631=ORIENTED_EDGE('',*,*,#10007,.F.);
#14632=ORIENTED_EDGE('',*,*,#9801,.T.);
#14633=ORIENTED_EDGE('',*,*,#10008,.F.);
#14634=ORIENTED_EDGE('',*,*,#9953,.T.);
#14635=ORIENTED_EDGE('',*,*,#10009,.T.);
#14636=ORIENTED_EDGE('',*,*,#9799,.T.);
#14637=ORIENTED_EDGE('',*,*,#10010,.T.);
#14638=ORIENTED_EDGE('',*,*,#9962,.T.);
#14639=ORIENTED_EDGE('',*,*,#10011,.F.);
#14640=ORIENTED_EDGE('',*,*,#9798,.T.);
#14641=ORIENTED_EDGE('',*,*,#9802,.T.);
#14642=ORIENTED_EDGE('',*,*,#10009,.F.);
#14643=ORIENTED_EDGE('',*,*,#9952,.T.);
#14644=ORIENTED_EDGE('',*,*,#9956,.T.);
#14645=ORIENTED_EDGE('',*,*,#10006,.F.);
#14646=ORIENTED_EDGE('',*,*,#9805,.T.);
#14647=ORIENTED_EDGE('',*,*,#9809,.T.);
#14648=ORIENTED_EDGE('',*,*,#10005,.F.);
#14649=ORIENTED_EDGE('',*,*,#9945,.T.);
#14650=ORIENTED_EDGE('',*,*,#9949,.T.);
#14651=ORIENTED_EDGE('',*,*,#10002,.F.);
#14652=ORIENTED_EDGE('',*,*,#9812,.T.);
#14653=ORIENTED_EDGE('',*,*,#9816,.T.);
#14654=ORIENTED_EDGE('',*,*,#10001,.F.);
#14655=ORIENTED_EDGE('',*,*,#9938,.T.);
#14656=ORIENTED_EDGE('',*,*,#9942,.T.);
#14657=ORIENTED_EDGE('',*,*,#9998,.F.);
#14658=ORIENTED_EDGE('',*,*,#9819,.T.);
#14659=ORIENTED_EDGE('',*,*,#9823,.T.);
#14660=ORIENTED_EDGE('',*,*,#9997,.F.);
#14661=ORIENTED_EDGE('',*,*,#9931,.T.);
#14662=ORIENTED_EDGE('',*,*,#9935,.T.);
#14663=ORIENTED_EDGE('',*,*,#9994,.F.);
#14664=ORIENTED_EDGE('',*,*,#9826,.T.);
#14665=ORIENTED_EDGE('',*,*,#9830,.T.);
#14666=ORIENTED_EDGE('',*,*,#9993,.F.);
#14667=ORIENTED_EDGE('',*,*,#9924,.T.);
#14668=ORIENTED_EDGE('',*,*,#9928,.T.);
#14669=ORIENTED_EDGE('',*,*,#9990,.F.);
#14670=ORIENTED_EDGE('',*,*,#9833,.T.);
#14671=ORIENTED_EDGE('',*,*,#10012,.T.);
#14672=ORIENTED_EDGE('',*,*,#10013,.T.);
#14673=ORIENTED_EDGE('',*,*,#10012,.F.);
#14674=ORIENTED_EDGE('',*,*,#9837,.T.);
#14675=ORIENTED_EDGE('',*,*,#9989,.F.);
#14676=ORIENTED_EDGE('',*,*,#9840,.T.);
#14677=ORIENTED_EDGE('',*,*,#9844,.T.);
#14678=ORIENTED_EDGE('',*,*,#9987,.F.);
#14679=ORIENTED_EDGE('',*,*,#9910,.T.);
#14680=ORIENTED_EDGE('',*,*,#9914,.T.);
#14681=ORIENTED_EDGE('',*,*,#9984,.F.);
#14682=ORIENTED_EDGE('',*,*,#9847,.T.);
#14683=ORIENTED_EDGE('',*,*,#9851,.T.);
#14684=ORIENTED_EDGE('',*,*,#9983,.F.);
#14685=ORIENTED_EDGE('',*,*,#9903,.T.);
#14686=ORIENTED_EDGE('',*,*,#9907,.T.);
#14687=ORIENTED_EDGE('',*,*,#9980,.F.);
#14688=ORIENTED_EDGE('',*,*,#9854,.T.);
#14689=ORIENTED_EDGE('',*,*,#9858,.T.);
#14690=ORIENTED_EDGE('',*,*,#9979,.F.);
#14691=ORIENTED_EDGE('',*,*,#9896,.T.);
#14692=ORIENTED_EDGE('',*,*,#9900,.T.);
#14693=ORIENTED_EDGE('',*,*,#9976,.F.);
#14694=ORIENTED_EDGE('',*,*,#9861,.T.);
#14695=ORIENTED_EDGE('',*,*,#9865,.T.);
#14696=ORIENTED_EDGE('',*,*,#9975,.F.);
#14697=ORIENTED_EDGE('',*,*,#9889,.T.);
#14698=ORIENTED_EDGE('',*,*,#9893,.T.);
#14699=ORIENTED_EDGE('',*,*,#9972,.F.);
#14700=ORIENTED_EDGE('',*,*,#9868,.T.);
#14701=ORIENTED_EDGE('',*,*,#9872,.T.);
#14702=ORIENTED_EDGE('',*,*,#9971,.F.);
#14703=ORIENTED_EDGE('',*,*,#9882,.T.);
#14704=ORIENTED_EDGE('',*,*,#9886,.T.);
#14705=ORIENTED_EDGE('',*,*,#9968,.F.);
#14706=ORIENTED_EDGE('',*,*,#9875,.T.);
#14707=ORIENTED_EDGE('',*,*,#9879,.T.);
#14708=ORIENTED_EDGE('',*,*,#9967,.F.);
#14709=ORIENTED_EDGE('',*,*,#9917,.T.);
#14710=ORIENTED_EDGE('',*,*,#9921,.T.);
#14711=ORIENTED_EDGE('',*,*,#9965,.F.);
#14712=ORIENTED_EDGE('',*,*,#9959,.T.);
#14713=ORIENTED_EDGE('',*,*,#9963,.T.);
#14714=ORIENTED_EDGE('',*,*,#10010,.F.);
#14715=ORIENTED_EDGE('',*,*,#10014,.F.);
#14716=ORIENTED_EDGE('',*,*,#9789,.F.);
#14717=ORIENTED_EDGE('',*,*,#9719,.F.);
#14718=ORIENTED_EDGE('',*,*,#9790,.F.);
#14719=ORIENTED_EDGE('',*,*,#10015,.T.);
#14720=ORIENTED_EDGE('',*,*,#10014,.T.);
#14721=ORIENTED_EDGE('',*,*,#10015,.F.);
#14722=ORIENTED_EDGE('',*,*,#9748,.T.);
#14723=ORIENTED_EDGE('',*,*,#9786,.T.);
#14724=ORIENTED_EDGE('',*,*,#10016,.F.);
#14725=ORIENTED_EDGE('',*,*,#9795,.T.);
#14726=ORIENTED_EDGE('',*,*,#10013,.F.);
#14727=ORIENTED_EDGE('',*,*,#10016,.T.);
#14728=ORIENTED_EDGE('',*,*,#9785,.T.);
#14729=ORIENTED_EDGE('',*,*,#9753,.T.);
#14730=ORIENTED_EDGE('',*,*,#9794,.T.);
#14731=ORIENTED_EDGE('',*,*,#10017,.F.);
#14732=ORIENTED_EDGE('',*,*,#10018,.T.);
#14733=ORIENTED_EDGE('',*,*,#9831,.T.);
#14734=ORIENTED_EDGE('',*,*,#9991,.T.);
#14735=ORIENTED_EDGE('',*,*,#9926,.T.);
#14736=ORIENTED_EDGE('',*,*,#9922,.T.);
#14737=ORIENTED_EDGE('',*,*,#9992,.T.);
#14738=ORIENTED_EDGE('',*,*,#9828,.T.);
#14739=ORIENTED_EDGE('',*,*,#9824,.T.);
#14740=ORIENTED_EDGE('',*,*,#9995,.T.);
#14741=ORIENTED_EDGE('',*,*,#9933,.T.);
#14742=ORIENTED_EDGE('',*,*,#9929,.T.);
#14743=ORIENTED_EDGE('',*,*,#9996,.T.);
#14744=ORIENTED_EDGE('',*,*,#9821,.T.);
#14745=ORIENTED_EDGE('',*,*,#9817,.T.);
#14746=ORIENTED_EDGE('',*,*,#9999,.T.);
#14747=ORIENTED_EDGE('',*,*,#9940,.T.);
#14748=ORIENTED_EDGE('',*,*,#9936,.T.);
#14749=ORIENTED_EDGE('',*,*,#10000,.T.);
#14750=ORIENTED_EDGE('',*,*,#9814,.T.);
#14751=ORIENTED_EDGE('',*,*,#9810,.T.);
#14752=ORIENTED_EDGE('',*,*,#10003,.T.);
#14753=ORIENTED_EDGE('',*,*,#9947,.T.);
#14754=ORIENTED_EDGE('',*,*,#9943,.T.);
#14755=ORIENTED_EDGE('',*,*,#10004,.T.);
#14756=ORIENTED_EDGE('',*,*,#9807,.T.);
#14757=ORIENTED_EDGE('',*,*,#9803,.T.);
#14758=ORIENTED_EDGE('',*,*,#10007,.T.);
#14759=ORIENTED_EDGE('',*,*,#9954,.T.);
#14760=ORIENTED_EDGE('',*,*,#9950,.T.);
#14761=ORIENTED_EDGE('',*,*,#10008,.T.);
#14762=ORIENTED_EDGE('',*,*,#9800,.T.);
#14763=ORIENTED_EDGE('',*,*,#9796,.T.);
#14764=ORIENTED_EDGE('',*,*,#10011,.T.);
#14765=ORIENTED_EDGE('',*,*,#9961,.T.);
#14766=ORIENTED_EDGE('',*,*,#9957,.T.);
#14767=ORIENTED_EDGE('',*,*,#9964,.T.);
#14768=ORIENTED_EDGE('',*,*,#9919,.T.);
#14769=ORIENTED_EDGE('',*,*,#9915,.T.);
#14770=ORIENTED_EDGE('',*,*,#9966,.T.);
#14771=ORIENTED_EDGE('',*,*,#9877,.T.);
#14772=ORIENTED_EDGE('',*,*,#9873,.T.);
#14773=ORIENTED_EDGE('',*,*,#9969,.T.);
#14774=ORIENTED_EDGE('',*,*,#9884,.T.);
#14775=ORIENTED_EDGE('',*,*,#9880,.T.);
#14776=ORIENTED_EDGE('',*,*,#9970,.T.);
#14777=ORIENTED_EDGE('',*,*,#9870,.T.);
#14778=ORIENTED_EDGE('',*,*,#9866,.T.);
#14779=ORIENTED_EDGE('',*,*,#9973,.T.);
#14780=ORIENTED_EDGE('',*,*,#9891,.T.);
#14781=ORIENTED_EDGE('',*,*,#9887,.T.);
#14782=ORIENTED_EDGE('',*,*,#9974,.T.);
#14783=ORIENTED_EDGE('',*,*,#9863,.T.);
#14784=ORIENTED_EDGE('',*,*,#9859,.T.);
#14785=ORIENTED_EDGE('',*,*,#9977,.T.);
#14786=ORIENTED_EDGE('',*,*,#9898,.T.);
#14787=ORIENTED_EDGE('',*,*,#9894,.T.);
#14788=ORIENTED_EDGE('',*,*,#9978,.T.);
#14789=ORIENTED_EDGE('',*,*,#9856,.T.);
#14790=ORIENTED_EDGE('',*,*,#9852,.T.);
#14791=ORIENTED_EDGE('',*,*,#9981,.T.);
#14792=ORIENTED_EDGE('',*,*,#9905,.T.);
#14793=ORIENTED_EDGE('',*,*,#9901,.T.);
#14794=ORIENTED_EDGE('',*,*,#9982,.T.);
#14795=ORIENTED_EDGE('',*,*,#9849,.T.);
#14796=ORIENTED_EDGE('',*,*,#9845,.T.);
#14797=ORIENTED_EDGE('',*,*,#9985,.T.);
#14798=ORIENTED_EDGE('',*,*,#9912,.T.);
#14799=ORIENTED_EDGE('',*,*,#9908,.T.);
#14800=ORIENTED_EDGE('',*,*,#9986,.T.);
#14801=ORIENTED_EDGE('',*,*,#9842,.T.);
#14802=ORIENTED_EDGE('',*,*,#9838,.T.);
#14803=ORIENTED_EDGE('',*,*,#9988,.T.);
#14804=ORIENTED_EDGE('',*,*,#9835,.T.);
#14805=ORIENTED_EDGE('',*,*,#10018,.F.);
#14806=ORIENTED_EDGE('',*,*,#10017,.T.);
#14807=PLANE('',#16405);
#14808=PLANE('',#16406);
#14809=PLANE('',#16407);
#14810=PLANE('',#16408);
#14811=PLANE('',#16409);
#14812=PLANE('',#16410);
#14813=PLANE('',#16411);
#14814=PLANE('',#16412);
#14815=PLANE('',#16413);
#14816=PLANE('',#16414);
#14817=PLANE('',#16415);
#14818=PLANE('',#16416);
#14819=PLANE('',#16417);
#14820=PLANE('',#16418);
#14821=PLANE('',#16419);
#14822=PLANE('',#16420);
#14823=PLANE('',#16421);
#14824=PLANE('',#16422);
#14825=PLANE('',#16423);
#14826=PLANE('',#16429);
#14827=PLANE('',#16436);
#14828=PLANE('',#16437);
#14829=PLANE('',#16438);
#14830=PLANE('',#16439);
#14831=PLANE('',#16440);
#14832=PLANE('',#16441);
#14833=PLANE('',#16442);
#14834=PLANE('',#16443);
#14835=PLANE('',#16447);
#14836=PLANE('',#16451);
#14837=PLANE('',#16452);
#14838=PLANE('',#16455);
#14839=PLANE('',#16458);
#14840=PLANE('',#16459);
#14841=PLANE('',#16463);
#14842=PLANE('',#16467);
#14843=PLANE('',#16468);
#14844=PLANE('',#16470);
#14845=PLANE('',#16472);
#14846=PLANE('',#16473);
#14847=PLANE('',#16477);
#14848=PLANE('',#16478);
#14849=PLANE('',#16479);
#14850=PLANE('',#16483);
#14851=PLANE('',#16484);
#14852=PLANE('',#16488);
#14853=PLANE('',#16492);
#14854=PLANE('',#16493);
#14855=PLANE('',#16497);
#14856=PLANE('',#16498);
#14857=PLANE('',#16499);
#14858=PLANE('',#16503);
#14859=PLANE('',#16504);
#14860=PLANE('',#16515);
#14861=PLANE('',#16516);
#14862=PLANE('',#16517);
#14863=PLANE('',#16521);
#14864=PLANE('',#16525);
#14865=PLANE('',#16526);
#14866=PLANE('',#16530);
#14867=PLANE('',#16531);
#14868=PLANE('',#16535);
#14869=PLANE('',#16536);
#14870=PLANE('',#16540);
#14871=PLANE('',#16541);
#14872=PLANE('',#16545);
#14873=PLANE('',#16548);
#14874=PLANE('',#16553);
#14875=PLANE('',#16554);
#14876=PLANE('',#16557);
#14877=PLANE('',#16558);
#14878=PLANE('',#16561);
#14879=PLANE('',#16564);
#14880=PLANE('',#16566);
#14881=PLANE('',#16570);
#14882=PLANE('',#16574);
#14883=PLANE('',#16576);
#14884=PLANE('',#16578);
#14885=PLANE('',#16579);
#14886=PLANE('',#16582);
#14887=PLANE('',#16593);
#14888=PLANE('',#16596);
#14889=PLANE('',#16597);
#14890=PLANE('',#16599);
#14891=PLANE('',#16603);
#14892=PLANE('',#16604);
#14893=PLANE('',#16610);
#14894=PLANE('',#16618);
#14895=PLANE('',#16624);
#14896=PLANE('',#16633);
#14897=PLANE('',#16648);
#14898=PLANE('',#16650);
#14899=PLANE('',#16651);
#14900=PLANE('',#16652);
#14901=PLANE('',#16653);
#14902=PLANE('',#16654);
#14903=PLANE('',#16655);
#14904=PLANE('',#16656);
#14905=PLANE('',#16657);
#14906=PLANE('',#16658);
#14907=PLANE('',#16659);
#14908=PLANE('',#16660);
#14909=PLANE('',#16661);
#14910=PLANE('',#16662);
#14911=PLANE('',#16663);
#14912=PLANE('',#16664);
#14913=PLANE('',#16665);
#14914=PLANE('',#16666);
#14915=PLANE('',#16667);
#14916=PLANE('',#16668);
#14917=PLANE('',#16669);
#14918=PLANE('',#16670);
#14919=PLANE('',#16671);
#14920=PLANE('',#16672);
#14921=PLANE('',#16673);
#14922=PLANE('',#16674);
#14923=PLANE('',#16675);
#14924=PLANE('',#16676);
#14925=PLANE('',#16677);
#14926=PLANE('',#16678);
#14927=PLANE('',#16679);
#14928=PLANE('',#16680);
#14929=PLANE('',#16681);
#14930=PLANE('',#16682);
#14931=PLANE('',#16683);
#14932=PLANE('',#16684);
#14933=PLANE('',#16691);
#14934=PLANE('',#16692);
#14935=PLANE('',#16693);
#14936=PLANE('',#16694);
#14937=PLANE('',#16695);
#14938=PLANE('',#16708);
#14939=PLANE('',#16714);
#14940=PLANE('',#16727);
#14941=PLANE('',#16736);
#14942=PLANE('',#16753);
#14943=PLANE('',#16764);
#14944=PLANE('',#16765);
#14945=PLANE('',#16766);
#14946=PLANE('',#16767);
#14947=PLANE('',#16771);
#14948=PLANE('',#16772);
#14949=PLANE('',#16773);
#14950=PLANE('',#16775);
#14951=PLANE('',#16783);
#14952=PLANE('',#16791);
#14953=PLANE('',#16793);
#14954=PLANE('',#16796);
#14955=PLANE('',#16801);
#14956=PLANE('',#16804);
#14957=PLANE('',#16805);
#14958=PLANE('',#16810);
#14959=PLANE('',#16813);
#14960=PLANE('',#16814);
#14961=PLANE('',#16816);
#14962=PLANE('',#16825);
#14963=PLANE('',#16827);
#14964=PLANE('',#16833);
#14965=PLANE('',#16849);
#14966=PLANE('',#16852);
#14967=PLANE('',#16857);
#14968=PLANE('',#16859);
#14969=PLANE('',#16861);
#14970=PLANE('',#16863);
#14971=PLANE('',#16865);
#14972=PLANE('',#16867);
#14973=PLANE('',#16877);
#14974=PLANE('',#16878);
#14975=PLANE('',#16879);
#14976=PLANE('',#16880);
#14977=PLANE('',#16881);
#14978=PLANE('',#16882);
#14979=PLANE('',#16883);
#14980=PLANE('',#16884);
#14981=PLANE('',#16885);
#14982=PLANE('',#16886);
#14983=PLANE('',#16887);
#14984=PLANE('',#16888);
#14985=PLANE('',#16889);
#14986=PLANE('',#16890);
#14987=PLANE('',#16891);
#14988=PLANE('',#16892);
#14989=PLANE('',#16893);
#14990=PLANE('',#16894);
#14991=PLANE('',#16895);
#14992=PLANE('',#16896);
#14993=PLANE('',#16897);
#14994=PLANE('',#16898);
#14995=PLANE('',#16899);
#14996=PLANE('',#16900);
#14997=PLANE('',#16901);
#14998=PLANE('',#16908);
#14999=PLANE('',#16923);
#15000=PLANE('',#16926);
#15001=PLANE('',#16931);
#15002=PLANE('',#16933);
#15003=PLANE('',#16935);
#15004=PLANE('',#16937);
#15005=PLANE('',#16939);
#15006=PLANE('',#16941);
#15007=PLANE('',#16951);
#15008=PLANE('',#16952);
#15009=PLANE('',#16953);
#15010=PLANE('',#16954);
#15011=PLANE('',#16955);
#15012=PLANE('',#16956);
#15013=PLANE('',#16957);
#15014=PLANE('',#16958);
#15015=PLANE('',#16959);
#15016=PLANE('',#16960);
#15017=PLANE('',#16961);
#15018=PLANE('',#16962);
#15019=PLANE('',#16963);
#15020=PLANE('',#16964);
#15021=PLANE('',#16965);
#15022=PLANE('',#16966);
#15023=PLANE('',#16967);
#15024=PLANE('',#16968);
#15025=PLANE('',#16969);
#15026=PLANE('',#16970);
#15027=PLANE('',#16971);
#15028=PLANE('',#16972);
#15029=PLANE('',#16973);
#15030=PLANE('',#16974);
#15031=PLANE('',#16975);
#15032=PLANE('',#16982);
#15033=PLANE('',#16984);
#15034=PLANE('',#16985);
#15035=PLANE('',#16986);
#15036=PLANE('',#16987);
#15037=PLANE('',#16988);
#15038=PLANE('',#16989);
#15039=PLANE('',#16990);
#15040=PLANE('',#16991);
#15041=PLANE('',#17011);
#15042=PLANE('',#17013);
#15043=PLANE('',#17014);
#15044=PLANE('',#17015);
#15045=PLANE('',#17016);
#15046=PLANE('',#17017);
#15047=PLANE('',#17018);
#15048=PLANE('',#17019);
#15049=PLANE('',#17020);
#15050=PLANE('',#17021);
#15051=PLANE('',#17022);
#15052=PLANE('',#17023);
#15053=PLANE('',#17024);
#15054=PLANE('',#17025);
#15055=PLANE('',#17026);
#15056=PLANE('',#17027);
#15057=PLANE('',#17028);
#15058=PLANE('',#17029);
#15059=PLANE('',#17030);
#15060=PLANE('',#17032);
#15061=PLANE('',#17033);
#15062=PLANE('',#17034);
#15063=PLANE('',#17035);
#15064=PLANE('',#17036);
#15065=PLANE('',#17037);
#15066=PLANE('',#17038);
#15067=PLANE('',#17039);
#15068=PLANE('',#17040);
#15069=PLANE('',#17041);
#15070=PLANE('',#17059);
#15071=PLANE('',#17063);
#15072=PLANE('',#17070);
#15073=PLANE('',#17074);
#15074=PLANE('',#17075);
#15075=PLANE('',#17076);
#15076=PLANE('',#17077);
#15077=PLANE('',#17078);
#15078=PLANE('',#17088);
#15079=PLANE('',#17089);
#15080=PLANE('',#17091);
#15081=PLANE('',#17092);
#15082=PLANE('',#17093);
#15083=PLANE('',#17094);
#15084=PLANE('',#17095);
#15085=PLANE('',#17096);
#15086=PLANE('',#17149);
#15087=PLANE('',#17150);
#15088=PLANE('',#17151);
#15089=PLANE('',#17152);
#15090=PLANE('',#17153);
#15091=PLANE('',#17157);
#15092=PLANE('',#17158);
#15093=PLANE('',#17163);
#15094=PLANE('',#17164);
#15095=PLANE('',#17165);
#15096=PLANE('',#17166);
#15097=PLANE('',#17167);
#15098=PLANE('',#17168);
#15099=PLANE('',#17169);
#15100=PLANE('',#17170);
#15101=PLANE('',#17171);
#15102=PLANE('',#17172);
#15103=PLANE('',#17173);
#15104=PLANE('',#17174);
#15105=PLANE('',#17175);
#15106=PLANE('',#17176);
#15107=PLANE('',#17177);
#15108=PLANE('',#17178);
#15109=PLANE('',#17179);
#15110=PLANE('',#17180);
#15111=PLANE('',#17181);
#15112=PLANE('',#17182);
#15113=PLANE('',#17183);
#15114=PLANE('',#17184);
#15115=PLANE('',#17185);
#15116=PLANE('',#17186);
#15117=PLANE('',#17187);
#15118=PLANE('',#17188);
#15119=PLANE('',#17189);
#15120=PLANE('',#17190);
#15121=PLANE('',#17191);
#15122=PLANE('',#17192);
#15123=PLANE('',#17193);
#15124=PLANE('',#17194);
#15125=PLANE('',#17195);
#15126=PLANE('',#17196);
#15127=PLANE('',#17197);
#15128=PLANE('',#17198);
#15129=PLANE('',#17199);
#15130=PLANE('',#17200);
#15131=PLANE('',#17201);
#15132=PLANE('',#17202);
#15133=PLANE('',#17203);
#15134=PLANE('',#17204);
#15135=PLANE('',#17205);
#15136=PLANE('',#17206);
#15137=PLANE('',#17207);
#15138=PLANE('',#17208);
#15139=PLANE('',#17209);
#15140=PLANE('',#17210);
#15141=PLANE('',#17211);
#15142=PLANE('',#17212);
#15143=PLANE('',#17213);
#15144=PLANE('',#17214);
#15145=PLANE('',#17215);
#15146=PLANE('',#17216);
#15147=PLANE('',#17217);
#15148=PLANE('',#17218);
#15149=PLANE('',#17219);
#15150=PLANE('',#17220);
#15151=PLANE('',#17221);
#15152=PLANE('',#17222);
#15153=PLANE('',#17315);
#15154=PLANE('',#17320);
#15155=PLANE('',#17323);
#15156=PLANE('',#17330);
#15157=PLANE('',#17331);
#15158=PLANE('',#17379);
#15159=PLANE('',#17382);
#15160=PLANE('',#17392);
#15161=PLANE('',#17429);
#15162=PLANE('',#17431);
#15163=PLANE('',#17433);
#15164=PLANE('',#17435);
#15165=PLANE('',#17437);
#15166=PLANE('',#17439);
#15167=PLANE('',#17449);
#15168=PLANE('',#17450);
#15169=PLANE('',#17451);
#15170=PLANE('',#17452);
#15171=PLANE('',#17453);
#15172=PLANE('',#17454);
#15173=PLANE('',#17455);
#15174=PLANE('',#17456);
#15175=PLANE('',#17457);
#15176=PLANE('',#17458);
#15177=PLANE('',#17459);
#15178=PLANE('',#17460);
#15179=PLANE('',#17461);
#15180=PLANE('',#17462);
#15181=PLANE('',#17463);
#15182=PLANE('',#17464);
#15183=PLANE('',#17465);
#15184=PLANE('',#17466);
#15185=PLANE('',#17467);
#15186=PLANE('',#17468);
#15187=PLANE('',#17469);
#15188=PLANE('',#17470);
#15189=PLANE('',#17471);
#15190=PLANE('',#17472);
#15191=PLANE('',#17473);
#15192=PLANE('',#17474);
#15193=PLANE('',#17475);
#15194=PLANE('',#17476);
#15195=PLANE('',#17477);
#15196=PLANE('',#17478);
#15197=PLANE('',#17479);
#15198=PLANE('',#17480);
#15199=PLANE('',#17481);
#15200=PLANE('',#17482);
#15201=PLANE('',#17483);
#15202=PLANE('',#17484);
#15203=PLANE('',#17485);
#15204=PLANE('',#17486);
#15205=PLANE('',#17487);
#15206=PLANE('',#17488);
#15207=PLANE('',#17489);
#15208=PLANE('',#17490);
#15209=PLANE('',#17491);
#15210=PLANE('',#17492);
#15211=PLANE('',#17493);
#15212=PLANE('',#17494);
#15213=PLANE('',#17495);
#15214=PLANE('',#17496);
#15215=PLANE('',#17497);
#15216=PLANE('',#17498);
#15217=PLANE('',#17499);
#15218=PLANE('',#17500);
#15219=PLANE('',#17501);
#15220=PLANE('',#17502);
#15221=PLANE('',#17503);
#15222=PLANE('',#17504);
#15223=PLANE('',#17505);
#15224=PLANE('',#17506);
#15225=PLANE('',#17507);
#15226=PLANE('',#17508);
#15227=PLANE('',#17509);
#15228=PLANE('',#17510);
#15229=PLANE('',#17511);
#15230=PLANE('',#17512);
#15231=PLANE('',#17513);
#15232=PLANE('',#17514);
#15233=PLANE('',#17515);
#15234=PLANE('',#17516);
#15235=PLANE('',#17517);
#15236=PLANE('',#17518);
#15237=PLANE('',#17519);
#15238=PLANE('',#17520);
#15239=PLANE('',#17521);
#15240=PLANE('',#17522);
#15241=PLANE('',#17523);
#15242=PLANE('',#17524);
#15243=PLANE('',#17525);
#15244=PLANE('',#17526);
#15245=PLANE('',#17527);
#15246=PLANE('',#17528);
#15247=PLANE('',#17529);
#15248=PLANE('',#17530);
#15249=PLANE('',#17531);
#15250=PLANE('',#17532);
#15251=PLANE('',#17533);
#15252=PLANE('',#17534);
#15253=PLANE('',#17535);
#15254=PLANE('',#17536);
#15255=PLANE('',#17537);
#15256=PLANE('',#17538);
#15257=PLANE('',#17539);
#15258=PLANE('',#17540);
#15259=PLANE('',#17541);
#15260=PLANE('',#17542);
#15261=PLANE('',#17543);
#15262=PLANE('',#17544);
#15263=PLANE('',#17617);
#15264=PLANE('',#17622);
#15265=PLANE('',#17648);
#15266=PLANE('',#17653);
#15267=PLANE('',#17654);
#15268=PLANE('',#17655);
#15269=PLANE('',#17656);
#15270=PLANE('',#17657);
#15271=PLANE('',#17658);
#15272=PLANE('',#17659);
#15273=PLANE('',#17660);
#15274=PLANE('',#17661);
#15275=PLANE('',#17662);
#15276=PLANE('',#17663);
#15277=PLANE('',#17664);
#15278=PLANE('',#17665);
#15279=PLANE('',#17666);
#15280=PLANE('',#17667);
#15281=PLANE('',#17668);
#15282=PLANE('',#17669);
#15283=PLANE('',#17670);
#15284=PLANE('',#17671);
#15285=PLANE('',#17672);
#15286=PLANE('',#17673);
#15287=PLANE('',#17674);
#15288=PLANE('',#17675);
#15289=PLANE('',#17676);
#15290=PLANE('',#17677);
#15291=PLANE('',#17678);
#15292=PLANE('',#17679);
#15293=PLANE('',#17680);
#15294=PLANE('',#17681);
#15295=PLANE('',#17682);
#15296=PLANE('',#17683);
#15297=PLANE('',#17684);
#15298=PLANE('',#17685);
#15299=PLANE('',#17686);
#15300=PLANE('',#17687);
#15301=PLANE('',#17688);
#15302=PLANE('',#17689);
#15303=PLANE('',#17690);
#15304=PLANE('',#17691);
#15305=PLANE('',#17692);
#15306=PLANE('',#17693);
#15307=PLANE('',#17694);
#15308=PLANE('',#17695);
#15309=PLANE('',#17696);
#15310=PLANE('',#17697);
#15311=PLANE('',#17698);
#15312=PLANE('',#17699);
#15313=PLANE('',#17700);
#15314=PLANE('',#17775);
#15315=PLANE('',#17780);
#15316=PLANE('',#17783);
#15317=ADVANCED_FACE('',(#1774),#14807,.T.);
#15318=ADVANCED_FACE('',(#1775),#14808,.T.);
#15319=ADVANCED_FACE('',(#1776),#14809,.T.);
#15320=ADVANCED_FACE('',(#1777),#14810,.T.);
#15321=ADVANCED_FACE('',(#1778),#14811,.T.);
#15322=ADVANCED_FACE('',(#1779),#14812,.T.);
#15323=ADVANCED_FACE('',(#1780),#14813,.T.);
#15324=ADVANCED_FACE('',(#1781),#14814,.T.);
#15325=ADVANCED_FACE('',(#1782),#14815,.T.);
#15326=ADVANCED_FACE('',(#1783),#14816,.T.);
#15327=ADVANCED_FACE('',(#1784),#14817,.T.);
#15328=ADVANCED_FACE('',(#1785),#14818,.T.);
#15329=ADVANCED_FACE('',(#1786),#14819,.T.);
#15330=ADVANCED_FACE('',(#1787),#14820,.T.);
#15331=ADVANCED_FACE('',(#1788),#14821,.T.);
#15332=ADVANCED_FACE('',(#1789),#14822,.T.);
#15333=ADVANCED_FACE('',(#1790),#14823,.T.);
#15334=ADVANCED_FACE('',(#1791),#14824,.T.);
#15335=ADVANCED_FACE('',(#1792),#14825,.T.);
#15336=ADVANCED_FACE('',(#1793),#1672,.F.);
#15337=ADVANCED_FACE('',(#1794),#1673,.F.);
#15338=ADVANCED_FACE('',(#1795,#1159),#14826,.T.);
#15339=ADVANCED_FACE('',(#1796),#1674,.F.);
#15340=ADVANCED_FACE('',(#1797,#1160),#877,.F.);
#15341=ADVANCED_FACE('',(#1798),#490,.T.);
#15342=ADVANCED_FACE('',(#1799),#878,.F.);
#15343=ADVANCED_FACE('',(#1800),#14827,.T.);
#15344=ADVANCED_FACE('',(#1801),#14828,.F.);
#15345=ADVANCED_FACE('',(#1802),#14829,.T.);
#15346=ADVANCED_FACE('',(#1803),#14830,.T.);
#15347=ADVANCED_FACE('',(#1804),#14831,.T.);
#15348=ADVANCED_FACE('',(#1805),#14832,.T.);
#15349=ADVANCED_FACE('',(#1806),#14833,.T.);
#15350=ADVANCED_FACE('',(#1807),#14834,.T.);
#15351=ADVANCED_FACE('',(#1808),#1675,.T.);
#15352=ADVANCED_FACE('',(#1809),#14835,.T.);
#15353=ADVANCED_FACE('',(#1810),#1676,.T.);
#15354=ADVANCED_FACE('',(#1811),#14836,.T.);
#15355=ADVANCED_FACE('',(#1812),#14837,.F.);
#15356=ADVANCED_FACE('',(#1813),#879,.T.);
#15357=ADVANCED_FACE('',(#1814),#14838,.T.);
#15358=ADVANCED_FACE('',(#1815),#880,.T.);
#15359=ADVANCED_FACE('',(#1816),#14839,.T.);
#15360=ADVANCED_FACE('',(#1817),#14840,.T.);
#15361=ADVANCED_FACE('',(#1818),#1677,.T.);
#15362=ADVANCED_FACE('',(#1819),#14841,.T.);
#15363=ADVANCED_FACE('',(#1820),#1678,.T.);
#15364=ADVANCED_FACE('',(#1821),#14842,.T.);
#15365=ADVANCED_FACE('',(#1822),#14843,.T.);
#15366=ADVANCED_FACE('',(#1823),#1679,.T.);
#15367=ADVANCED_FACE('',(#1824),#14844,.T.);
#15368=ADVANCED_FACE('',(#1825),#1680,.T.);
#15369=ADVANCED_FACE('',(#1826),#14845,.T.);
#15370=ADVANCED_FACE('',(#1827),#14846,.T.);
#15371=ADVANCED_FACE('',(#1828),#1681,.F.);
#15372=ADVANCED_FACE('',(#1829),#14847,.T.);
#15373=ADVANCED_FACE('',(#1830),#14848,.T.);
#15374=ADVANCED_FACE('',(#1831),#14849,.T.);
#15375=ADVANCED_FACE('',(#1832),#1682,.F.);
#15376=ADVANCED_FACE('',(#1833),#14850,.T.);
#15377=ADVANCED_FACE('',(#1834),#14851,.T.);
#15378=ADVANCED_FACE('',(#1835),#1683,.T.);
#15379=ADVANCED_FACE('',(#1836),#14852,.T.);
#15380=ADVANCED_FACE('',(#1837),#1684,.T.);
#15381=ADVANCED_FACE('',(#1838),#14853,.T.);
#15382=ADVANCED_FACE('',(#1839),#14854,.T.);
#15383=ADVANCED_FACE('',(#1840),#1685,.F.);
#15384=ADVANCED_FACE('',(#1841),#14855,.T.);
#15385=ADVANCED_FACE('',(#1842),#14856,.T.);
#15386=ADVANCED_FACE('',(#1843),#14857,.T.);
#15387=ADVANCED_FACE('',(#1844),#1686,.F.);
#15388=ADVANCED_FACE('',(#1845),#14858,.T.);
#15389=ADVANCED_FACE('',(#1846,#1161),#14859,.T.);
#15390=ADVANCED_FACE('',(#1847),#491,.T.);
#15391=ADVANCED_FACE('',(#1848,#1162),#881,.T.);
#15392=ADVANCED_FACE('',(#1849),#1687,.T.);
#15393=ADVANCED_FACE('',(#1850),#1688,.T.);
#15394=ADVANCED_FACE('',(#1851),#488,.F.);
#15395=ADVANCED_FACE('',(#1852),#14860,.T.);
#15396=ADVANCED_FACE('',(#1853),#14861,.T.);
#15397=ADVANCED_FACE('',(#1854),#14862,.T.);
#15398=ADVANCED_FACE('',(#1855),#1689,.T.);
#15399=ADVANCED_FACE('',(#1856),#14863,.T.);
#15400=ADVANCED_FACE('',(#1857),#1690,.T.);
#15401=ADVANCED_FACE('',(#1858),#14864,.T.);
#15402=ADVANCED_FACE('',(#1859),#14865,.T.);
#15403=ADVANCED_FACE('',(#1860),#1691,.F.);
#15404=ADVANCED_FACE('',(#1861),#14866,.T.);
#15405=ADVANCED_FACE('',(#1862),#14867,.T.);
#15406=ADVANCED_FACE('',(#1863),#1692,.F.);
#15407=ADVANCED_FACE('',(#1864),#14868,.T.);
#15408=ADVANCED_FACE('',(#1865),#14869,.T.);
#15409=ADVANCED_FACE('',(#1866),#1693,.F.);
#15410=ADVANCED_FACE('',(#1867),#14870,.T.);
#15411=ADVANCED_FACE('',(#1868),#14871,.T.);
#15412=ADVANCED_FACE('',(#1869),#1694,.F.);
#15413=ADVANCED_FACE('',(#1870),#14872,.T.);
#15414=ADVANCED_FACE('',(#1871),#1695,.T.);
#15415=ADVANCED_FACE('',(#1872),#14873,.T.);
#15416=ADVANCED_FACE('',(#1873),#1696,.T.);
#15417=ADVANCED_FACE('',(#1874),#882,.F.);
#15418=ADVANCED_FACE('',(#1875),#14874,.F.);
#15419=ADVANCED_FACE('',(#1876),#14875,.F.);
#15420=ADVANCED_FACE('',(#1877),#883,.F.);
#15421=ADVANCED_FACE('',(#1878),#14876,.F.);
#15422=ADVANCED_FACE('',(#1879),#14877,.F.);
#15423=ADVANCED_FACE('',(#1880),#1697,.T.);
#15424=ADVANCED_FACE('',(#1881),#14878,.T.);
#15425=ADVANCED_FACE('',(#1882),#1698,.T.);
#15426=ADVANCED_FACE('',(#1883),#14879,.T.);
#15427=ADVANCED_FACE('',(#1884),#1699,.F.);
#15428=ADVANCED_FACE('',(#1885),#14880,.T.);
#15429=ADVANCED_FACE('',(#1886),#1700,.F.);
#15430=ADVANCED_FACE('',(#1887),#1701,.F.);
#15431=ADVANCED_FACE('',(#1888),#14881,.T.);
#15432=ADVANCED_FACE('',(#1889),#1702,.F.);
#15433=ADVANCED_FACE('',(#1890),#884,.T.);
#15434=ADVANCED_FACE('',(#1891),#14882,.T.);
#15435=ADVANCED_FACE('',(#1892),#885,.T.);
#15436=ADVANCED_FACE('',(#1893),#14883,.F.);
#15437=ADVANCED_FACE('',(#1894),#886,.F.);
#15438=ADVANCED_FACE('',(#1895),#14884,.F.);
#15439=ADVANCED_FACE('',(#1896),#14885,.F.);
#15440=ADVANCED_FACE('',(#1897),#887,.F.);
#15441=ADVANCED_FACE('',(#1898,#1163),#14886,.F.);
#15442=ADVANCED_FACE('',(#1899),#1703,.F.);
#15443=ADVANCED_FACE('',(#1900),#888,.F.);
#15444=ADVANCED_FACE('',(#1901),#1704,.F.);
#15445=ADVANCED_FACE('',(#1902,#1164),#14887,.F.);
#15446=ADVANCED_FACE('',(#1903),#889,.F.);
#15447=ADVANCED_FACE('',(#1904),#14888,.F.);
#15448=ADVANCED_FACE('',(#1905),#14889,.F.);
#15449=ADVANCED_FACE('',(#1906),#890,.F.);
#15450=ADVANCED_FACE('',(#1907),#14890,.F.);
#15451=ADVANCED_FACE('',(#1908),#891,.F.);
#15452=ADVANCED_FACE('',(#1909),#14891,.F.);
#15453=ADVANCED_FACE('',(#1910),#14892,.T.);
#15454=ADVANCED_FACE('',(#1911),#1705,.T.);
#15455=ADVANCED_FACE('',(#1912),#892,.T.);
#15456=ADVANCED_FACE('',(#1913,#1165),#14893,.T.);
#15457=ADVANCED_FACE('',(#1914),#1706,.T.);
#15458=ADVANCED_FACE('',(#1915,#1166),#893,.T.);
#15459=ADVANCED_FACE('',(#1916),#1707,.T.);
#15460=ADVANCED_FACE('',(#1917,#1167),#14894,.T.);
#15461=ADVANCED_FACE('',(#1918),#1708,.F.);
#15462=ADVANCED_FACE('',(#1919,#1168),#894,.F.);
#15463=ADVANCED_FACE('',(#1920),#14895,.T.);
#15464=ADVANCED_FACE('',(#1921),#1709,.T.);
#15465=ADVANCED_FACE('',(#1922),#1710,.T.);
#15466=ADVANCED_FACE('',(#1923),#14896,.T.);
#15467=ADVANCED_FACE('',(#1924),#1711,.T.);
#15468=ADVANCED_FACE('',(#1925),#895,.T.);
#15469=ADVANCED_FACE('',(#1926),#1712,.T.);
#15470=ADVANCED_FACE('',(#1927),#1713,.T.);
#15471=ADVANCED_FACE('',(#1928),#1714,.T.);
#15472=ADVANCED_FACE('',(#1929),#14897,.T.);
#15473=ADVANCED_FACE('',(#1930),#14898,.T.);
#15474=ADVANCED_FACE('',(#1931),#14899,.T.);
#15475=ADVANCED_FACE('',(#1932),#14900,.T.);
#15476=ADVANCED_FACE('',(#1933),#14901,.T.);
#15477=ADVANCED_FACE('',(#1934),#14902,.T.);
#15478=ADVANCED_FACE('',(#1935),#14903,.T.);
#15479=ADVANCED_FACE('',(#1936),#14904,.T.);
#15480=ADVANCED_FACE('',(#1937),#14905,.T.);
#15481=ADVANCED_FACE('',(#1938),#14906,.T.);
#15482=ADVANCED_FACE('',(#1939),#14907,.T.);
#15483=ADVANCED_FACE('',(#1940),#14908,.T.);
#15484=ADVANCED_FACE('',(#1941),#14909,.T.);
#15485=ADVANCED_FACE('',(#1942),#14910,.T.);
#15486=ADVANCED_FACE('',(#1943),#14911,.T.);
#15487=ADVANCED_FACE('',(#1944),#14912,.T.);
#15488=ADVANCED_FACE('',(#1945),#14913,.T.);
#15489=ADVANCED_FACE('',(#1946),#14914,.T.);
#15490=ADVANCED_FACE('',(#1947),#14915,.T.);
#15491=ADVANCED_FACE('',(#1948),#14916,.T.);
#15492=ADVANCED_FACE('',(#1949),#14917,.T.);
#15493=ADVANCED_FACE('',(#1950),#14918,.T.);
#15494=ADVANCED_FACE('',(#1951),#14919,.T.);
#15495=ADVANCED_FACE('',(#1952),#14920,.T.);
#15496=ADVANCED_FACE('',(#1953),#14921,.T.);
#15497=ADVANCED_FACE('',(#1954),#14922,.T.);
#15498=ADVANCED_FACE('',(#1955),#14923,.T.);
#15499=ADVANCED_FACE('',(#1956),#14924,.T.);
#15500=ADVANCED_FACE('',(#1957),#14925,.T.);
#15501=ADVANCED_FACE('',(#1958),#14926,.T.);
#15502=ADVANCED_FACE('',(#1959),#14927,.T.);
#15503=ADVANCED_FACE('',(#1960),#14928,.T.);
#15504=ADVANCED_FACE('',(#1961),#14929,.T.);
#15505=ADVANCED_FACE('',(#1962),#14930,.T.);
#15506=ADVANCED_FACE('',(#1963),#14931,.T.);
#15507=ADVANCED_FACE('',(#1964,#1169,#1170,#1171,#1172,#1173,#1174),#14932,
 .T.);
#15508=ADVANCED_FACE('',(#1965),#14933,.T.);
#15509=ADVANCED_FACE('',(#1966),#14934,.T.);
#15510=ADVANCED_FACE('',(#1967),#14935,.T.);
#15511=ADVANCED_FACE('',(#1968),#14936,.T.);
#15512=ADVANCED_FACE('',(#1969),#14937,.T.);
#15513=ADVANCED_FACE('',(#1970),#1715,.F.);
#15514=ADVANCED_FACE('',(#1971),#896,.F.);
#15515=ADVANCED_FACE('',(#1972),#1716,.F.);
#15516=ADVANCED_FACE('',(#1973),#1717,.F.);
#15517=ADVANCED_FACE('',(#1974,#1175),#14938,.F.);
#15518=ADVANCED_FACE('',(#1975),#1718,.F.);
#15519=ADVANCED_FACE('',(#1976,#1176),#14939,.F.);
#15520=ADVANCED_FACE('',(#1977),#897,.F.);
#15521=ADVANCED_FACE('',(#1978),#1719,.F.);
#15522=ADVANCED_FACE('',(#1979),#898,.F.);
#15523=ADVANCED_FACE('',(#1980),#1720,.F.);
#15524=ADVANCED_FACE('',(#1981),#899,.F.);
#15525=ADVANCED_FACE('',(#1982),#1721,.F.);
#15526=ADVANCED_FACE('',(#1983,#1177),#14940,.F.);
#15527=ADVANCED_FACE('',(#1984),#1722,.F.);
#15528=ADVANCED_FACE('',(#1985),#900,.F.);
#15529=ADVANCED_FACE('',(#1986),#1723,.F.);
#15530=ADVANCED_FACE('',(#1987,#1178),#14941,.F.);
#15531=ADVANCED_FACE('',(#1988),#1724,.F.);
#15532=ADVANCED_FACE('',(#1989),#901,.F.);
#15533=ADVANCED_FACE('',(#1990),#1725,.F.);
#15534=ADVANCED_FACE('',(#1991),#902,.F.);
#15535=ADVANCED_FACE('',(#1992),#1726,.F.);
#15536=ADVANCED_FACE('',(#1993),#903,.F.);
#15537=ADVANCED_FACE('',(#1994),#1727,.F.);
#15538=ADVANCED_FACE('',(#1995,#1179,#1180,#1181,#1182,#1183,#1184),#14942,
 .F.);
#15539=ADVANCED_FACE('',(#1996),#904,.F.);
#15540=ADVANCED_FACE('',(#1997),#1728,.F.);
#15541=ADVANCED_FACE('',(#1998),#905,.F.);
#15542=ADVANCED_FACE('',(#1999),#1729,.F.);
#15543=ADVANCED_FACE('',(#2000),#14943,.T.);
#15544=ADVANCED_FACE('',(#2001),#14944,.T.);
#15545=ADVANCED_FACE('',(#2002),#14945,.T.);
#15546=ADVANCED_FACE('',(#2003),#14946,.T.);
#15547=ADVANCED_FACE('',(#2004),#1730,.F.);
#15548=ADVANCED_FACE('',(#2005),#1731,.F.);
#15549=ADVANCED_FACE('',(#2006),#1732,.F.);
#15550=ADVANCED_FACE('',(#2007),#14947,.T.);
#15551=ADVANCED_FACE('',(#2008),#14948,.T.);
#15552=ADVANCED_FACE('',(#2009),#14949,.T.);
#15553=ADVANCED_FACE('',(#2010),#14950,.T.);
#15554=ADVANCED_FACE('',(#2011),#1733,.T.);
#15555=ADVANCED_FACE('',(#2012),#906,.T.);
#15556=ADVANCED_FACE('',(#2013),#1734,.T.);
#15557=ADVANCED_FACE('',(#2014),#14951,.T.);
#15558=ADVANCED_FACE('',(#2015),#907,.T.);
#15559=ADVANCED_FACE('',(#2016),#908,.T.);
#15560=ADVANCED_FACE('',(#2017),#909,.T.);
#15561=ADVANCED_FACE('',(#2018),#910,.T.);
#15562=ADVANCED_FACE('',(#2019),#492,.F.);
#15563=ADVANCED_FACE('',(#2020),#14952,.F.);
#15564=ADVANCED_FACE('',(#2021),#14953,.F.);
#15565=ADVANCED_FACE('',(#2022),#14954,.F.);
#15566=ADVANCED_FACE('',(#2023),#493,.F.);
#15567=ADVANCED_FACE('',(#2024),#494,.F.);
#15568=ADVANCED_FACE('',(#2025),#495,.F.);
#15569=ADVANCED_FACE('',(#2026),#911,.T.);
#15570=ADVANCED_FACE('',(#2027),#912,.T.);
#15571=ADVANCED_FACE('',(#2028),#14955,.T.);
#15572=ADVANCED_FACE('',(#2029),#496,.F.);
#15573=ADVANCED_FACE('',(#2030),#14956,.F.);
#15574=ADVANCED_FACE('',(#2031),#14957,.F.);
#15575=ADVANCED_FACE('',(#2032),#913,.T.);
#15576=ADVANCED_FACE('',(#2033),#914,.T.);
#15577=ADVANCED_FACE('',(#2034),#14958,.F.);
#15578=ADVANCED_FACE('',(#2035),#14959,.F.);
#15579=ADVANCED_FACE('',(#2036),#14960,.F.);
#15580=ADVANCED_FACE('',(#2037),#14961,.F.);
#15581=ADVANCED_FACE('',(#2038),#915,.F.);
#15582=ADVANCED_FACE('',(#2039),#1735,.T.);
#15583=ADVANCED_FACE('',(#2040),#1736,.T.);
#15584=ADVANCED_FACE('',(#2041),#14962,.T.);
#15585=ADVANCED_FACE('',(#2042),#14963,.T.);
#15586=ADVANCED_FACE('',(#2043),#1737,.F.);
#15587=ADVANCED_FACE('',(#2044),#1738,.F.);
#15588=ADVANCED_FACE('',(#2045),#1739,.T.);
#15589=ADVANCED_FACE('',(#2046,#1185),#14964,.T.);
#15590=ADVANCED_FACE('',(#2047),#916,.T.);
#15591=ADVANCED_FACE('',(#2048),#917,.T.);
#15592=ADVANCED_FACE('',(#2049),#918,.T.);
#15593=ADVANCED_FACE('',(#2050),#919,.T.);
#15594=ADVANCED_FACE('',(#2051),#920,.T.);
#15595=ADVANCED_FACE('',(#2052),#921,.T.);
#15596=ADVANCED_FACE('',(#2053),#922,.T.);
#15597=ADVANCED_FACE('',(#2054),#923,.T.);
#15598=ADVANCED_FACE('',(#2055),#924,.T.);
#15599=ADVANCED_FACE('',(#2056),#925,.T.);
#15600=ADVANCED_FACE('',(#2057),#926,.T.);
#15601=ADVANCED_FACE('',(#2058),#927,.T.);
#15602=ADVANCED_FACE('',(#2059),#14965,.F.);
#15603=ADVANCED_FACE('',(#2060),#497,.F.);
#15604=ADVANCED_FACE('',(#2061),#14966,.T.);
#15605=ADVANCED_FACE('',(#2062),#928,.T.);
#15606=ADVANCED_FACE('',(#2063),#498,.F.);
#15607=ADVANCED_FACE('',(#2064),#14967,.F.);
#15608=ADVANCED_FACE('',(#2065),#14968,.F.);
#15609=ADVANCED_FACE('',(#2066),#14969,.F.);
#15610=ADVANCED_FACE('',(#2067),#14970,.F.);
#15611=ADVANCED_FACE('',(#2068),#14971,.F.);
#15612=ADVANCED_FACE('',(#2069),#14972,.F.);
#15613=ADVANCED_FACE('',(#2070),#1740,.F.);
#15614=ADVANCED_FACE('',(#2071),#14973,.F.);
#15615=ADVANCED_FACE('',(#2072),#14974,.F.);
#15616=ADVANCED_FACE('',(#2073),#14975,.F.);
#15617=ADVANCED_FACE('',(#2074),#14976,.F.);
#15618=ADVANCED_FACE('',(#2075),#14977,.F.);
#15619=ADVANCED_FACE('',(#2076),#14978,.F.);
#15620=ADVANCED_FACE('',(#2077),#14979,.F.);
#15621=ADVANCED_FACE('',(#2078),#14980,.F.);
#15622=ADVANCED_FACE('',(#2079),#14981,.F.);
#15623=ADVANCED_FACE('',(#2080),#14982,.F.);
#15624=ADVANCED_FACE('',(#2081),#14983,.F.);
#15625=ADVANCED_FACE('',(#2082),#14984,.F.);
#15626=ADVANCED_FACE('',(#2083),#14985,.F.);
#15627=ADVANCED_FACE('',(#2084),#14986,.F.);
#15628=ADVANCED_FACE('',(#2085),#14987,.F.);
#15629=ADVANCED_FACE('',(#2086),#14988,.F.);
#15630=ADVANCED_FACE('',(#2087),#14989,.F.);
#15631=ADVANCED_FACE('',(#2088),#14990,.F.);
#15632=ADVANCED_FACE('',(#2089),#14991,.F.);
#15633=ADVANCED_FACE('',(#2090),#14992,.F.);
#15634=ADVANCED_FACE('',(#2091),#14993,.F.);
#15635=ADVANCED_FACE('',(#2092),#14994,.F.);
#15636=ADVANCED_FACE('',(#2093),#14995,.F.);
#15637=ADVANCED_FACE('',(#2094),#14996,.F.);
#15638=ADVANCED_FACE('',(#2095),#14997,.T.);
#15639=ADVANCED_FACE('',(#2096),#1741,.T.);
#15640=ADVANCED_FACE('',(#2097),#929,.T.);
#15641=ADVANCED_FACE('',(#2098),#1742,.T.);
#15642=ADVANCED_FACE('',(#2099,#1186),#14998,.T.);
#15643=ADVANCED_FACE('',(#2100),#930,.T.);
#15644=ADVANCED_FACE('',(#2101),#931,.T.);
#15645=ADVANCED_FACE('',(#2102),#932,.T.);
#15646=ADVANCED_FACE('',(#2103),#933,.T.);
#15647=ADVANCED_FACE('',(#2104),#934,.T.);
#15648=ADVANCED_FACE('',(#2105),#935,.T.);
#15649=ADVANCED_FACE('',(#2106),#936,.T.);
#15650=ADVANCED_FACE('',(#2107),#937,.T.);
#15651=ADVANCED_FACE('',(#2108),#938,.T.);
#15652=ADVANCED_FACE('',(#2109),#939,.T.);
#15653=ADVANCED_FACE('',(#2110),#14999,.F.);
#15654=ADVANCED_FACE('',(#2111),#499,.F.);
#15655=ADVANCED_FACE('',(#2112),#15000,.T.);
#15656=ADVANCED_FACE('',(#2113),#940,.T.);
#15657=ADVANCED_FACE('',(#2114),#500,.F.);
#15658=ADVANCED_FACE('',(#2115),#15001,.F.);
#15659=ADVANCED_FACE('',(#2116),#15002,.F.);
#15660=ADVANCED_FACE('',(#2117),#15003,.F.);
#15661=ADVANCED_FACE('',(#2118),#15004,.F.);
#15662=ADVANCED_FACE('',(#2119),#15005,.F.);
#15663=ADVANCED_FACE('',(#2120),#15006,.F.);
#15664=ADVANCED_FACE('',(#2121),#1743,.F.);
#15665=ADVANCED_FACE('',(#2122),#15007,.F.);
#15666=ADVANCED_FACE('',(#2123),#15008,.F.);
#15667=ADVANCED_FACE('',(#2124),#15009,.F.);
#15668=ADVANCED_FACE('',(#2125),#15010,.F.);
#15669=ADVANCED_FACE('',(#2126),#15011,.F.);
#15670=ADVANCED_FACE('',(#2127),#15012,.F.);
#15671=ADVANCED_FACE('',(#2128),#15013,.F.);
#15672=ADVANCED_FACE('',(#2129),#15014,.F.);
#15673=ADVANCED_FACE('',(#2130),#15015,.F.);
#15674=ADVANCED_FACE('',(#2131),#15016,.F.);
#15675=ADVANCED_FACE('',(#2132),#15017,.F.);
#15676=ADVANCED_FACE('',(#2133),#15018,.F.);
#15677=ADVANCED_FACE('',(#2134),#15019,.F.);
#15678=ADVANCED_FACE('',(#2135),#15020,.F.);
#15679=ADVANCED_FACE('',(#2136),#15021,.F.);
#15680=ADVANCED_FACE('',(#2137),#15022,.F.);
#15681=ADVANCED_FACE('',(#2138),#15023,.F.);
#15682=ADVANCED_FACE('',(#2139),#15024,.F.);
#15683=ADVANCED_FACE('',(#2140),#15025,.F.);
#15684=ADVANCED_FACE('',(#2141),#15026,.F.);
#15685=ADVANCED_FACE('',(#2142),#15027,.F.);
#15686=ADVANCED_FACE('',(#2143),#15028,.F.);
#15687=ADVANCED_FACE('',(#2144),#15029,.F.);
#15688=ADVANCED_FACE('',(#2145),#15030,.F.);
#15689=ADVANCED_FACE('',(#2146),#15031,.T.);
#15690=ADVANCED_FACE('',(#2147),#1744,.T.);
#15691=ADVANCED_FACE('',(#2148),#941,.T.);
#15692=ADVANCED_FACE('',(#2149),#1745,.T.);
#15693=ADVANCED_FACE('',(#2150,#1187),#15032,.T.);
#15694=ADVANCED_FACE('',(#2151),#15033,.T.);
#15695=ADVANCED_FACE('',(#2152),#15034,.T.);
#15696=ADVANCED_FACE('',(#2153),#15035,.T.);
#15697=ADVANCED_FACE('',(#2154),#15036,.T.);
#15698=ADVANCED_FACE('',(#2155),#15037,.T.);
#15699=ADVANCED_FACE('',(#2156),#15038,.T.);
#15700=ADVANCED_FACE('',(#2157),#15039,.T.);
#15701=ADVANCED_FACE('',(#2158),#15040,.T.);
#15702=ADVANCED_FACE('',(#2159),#501,.T.);
#15703=ADVANCED_FACE('',(#2160,#1188),#942,.T.);
#15704=ADVANCED_FACE('',(#2161),#943,.F.);
#15705=ADVANCED_FACE('',(#2162),#1746,.T.);
#15706=ADVANCED_FACE('',(#2163),#1747,.T.);
#15707=ADVANCED_FACE('',(#2164),#1748,.T.);
#15708=ADVANCED_FACE('',(#2165),#502,.T.);
#15709=ADVANCED_FACE('',(#2166,#1189),#944,.F.);
#15710=ADVANCED_FACE('',(#2167),#1749,.T.);
#15711=ADVANCED_FACE('',(#2168,#1190),#15041,.F.);
#15712=ADVANCED_FACE('',(#2169),#15042,.T.);
#15713=ADVANCED_FACE('',(#2170),#15043,.T.);
#15714=ADVANCED_FACE('',(#2171),#15044,.T.);
#15715=ADVANCED_FACE('',(#2172),#15045,.T.);
#15716=ADVANCED_FACE('',(#2173),#15046,.T.);
#15717=ADVANCED_FACE('',(#2174),#15047,.T.);
#15718=ADVANCED_FACE('',(#2175),#15048,.T.);
#15719=ADVANCED_FACE('',(#2176),#15049,.T.);
#15720=ADVANCED_FACE('',(#2177),#15050,.T.);
#15721=ADVANCED_FACE('',(#2178),#15051,.T.);
#15722=ADVANCED_FACE('',(#2179),#15052,.T.);
#15723=ADVANCED_FACE('',(#2180),#15053,.T.);
#15724=ADVANCED_FACE('',(#2181),#15054,.T.);
#15725=ADVANCED_FACE('',(#2182),#15055,.T.);
#15726=ADVANCED_FACE('',(#2183),#15056,.T.);
#15727=ADVANCED_FACE('',(#2184),#15057,.T.);
#15728=ADVANCED_FACE('',(#2185),#15058,.T.);
#15729=ADVANCED_FACE('',(#2186),#15059,.T.);
#15730=ADVANCED_FACE('',(#2187),#15060,.T.);
#15731=ADVANCED_FACE('',(#2188),#15061,.T.);
#15732=ADVANCED_FACE('',(#2189),#15062,.T.);
#15733=ADVANCED_FACE('',(#2190),#15063,.T.);
#15734=ADVANCED_FACE('',(#2191),#15064,.T.);
#15735=ADVANCED_FACE('',(#2192),#15065,.T.);
#15736=ADVANCED_FACE('',(#2193),#15066,.T.);
#15737=ADVANCED_FACE('',(#2194),#15067,.F.);
#15738=ADVANCED_FACE('',(#2195),#15068,.F.);
#15739=ADVANCED_FACE('',(#2196,#1191,#1192,#1193,#1194,#1195),#15069,.T.);
#15740=ADVANCED_FACE('',(#2197),#1750,.F.);
#15741=ADVANCED_FACE('',(#2198),#1751,.F.);
#15742=ADVANCED_FACE('',(#2199),#1752,.F.);
#15743=ADVANCED_FACE('',(#2200),#945,.F.);
#15744=ADVANCED_FACE('',(#2201),#1753,.F.);
#15745=ADVANCED_FACE('',(#2202),#946,.F.);
#15746=ADVANCED_FACE('',(#2203),#1754,.F.);
#15747=ADVANCED_FACE('',(#2204),#15070,.T.);
#15748=ADVANCED_FACE('',(#2205),#1755,.F.);
#15749=ADVANCED_FACE('',(#2206),#15071,.T.);
#15750=ADVANCED_FACE('',(#2207),#1756,.F.);
#15751=ADVANCED_FACE('',(#2208),#1757,.F.);
#15752=ADVANCED_FACE('',(#2209),#1758,.F.);
#15753=ADVANCED_FACE('',(#2210,#1196,#1197,#1198),#15072,.T.);
#15754=ADVANCED_FACE('',(#2211),#1759,.F.);
#15755=ADVANCED_FACE('',(#2212),#15073,.T.);
#15756=ADVANCED_FACE('',(#2213),#15074,.T.);
#15757=ADVANCED_FACE('',(#2214),#15075,.T.);
#15758=ADVANCED_FACE('',(#2215),#15076,.T.);
#15759=ADVANCED_FACE('',(#2216),#15077,.T.);
#15760=ADVANCED_FACE('',(#2217),#1760,.F.);
#15761=ADVANCED_FACE('',(#2218),#947,.F.);
#15762=ADVANCED_FACE('',(#2219),#1761,.F.);
#15763=ADVANCED_FACE('',(#2220),#1762,.F.);
#15764=ADVANCED_FACE('',(#2221),#1763,.F.);
#15765=ADVANCED_FACE('',(#2222),#15078,.F.);
#15766=ADVANCED_FACE('',(#2223),#15079,.T.);
#15767=ADVANCED_FACE('',(#2224),#1764,.F.);
#15768=ADVANCED_FACE('',(#2225),#15080,.F.);
#15769=ADVANCED_FACE('',(#2226),#15081,.T.);
#15770=ADVANCED_FACE('',(#2227),#15082,.T.);
#15771=ADVANCED_FACE('',(#2228),#15083,.T.);
#15772=ADVANCED_FACE('',(#2229),#15084,.T.);
#15773=ADVANCED_FACE('',(#2230),#15085,.T.);
#15774=ADVANCED_FACE('',(#2231),#948,.F.);
#15775=ADVANCED_FACE('',(#2232),#949,.T.);
#15776=ADVANCED_FACE('',(#2233),#950,.T.);
#15777=ADVANCED_FACE('',(#2234),#951,.T.);
#15778=ADVANCED_FACE('',(#2235),#952,.T.);
#15779=ADVANCED_FACE('',(#2236),#953,.T.);
#15780=ADVANCED_FACE('',(#2237),#954,.T.);
#15781=ADVANCED_FACE('',(#2238),#955,.T.);
#15782=ADVANCED_FACE('',(#2239),#956,.T.);
#15783=ADVANCED_FACE('',(#2240),#957,.T.);
#15784=ADVANCED_FACE('',(#2241),#958,.T.);
#15785=ADVANCED_FACE('',(#2242),#959,.T.);
#15786=ADVANCED_FACE('',(#2243),#960,.T.);
#15787=ADVANCED_FACE('',(#2244),#961,.T.);
#15788=ADVANCED_FACE('',(#2245),#962,.T.);
#15789=ADVANCED_FACE('',(#2246),#963,.T.);
#15790=ADVANCED_FACE('',(#2247),#964,.T.);
#15791=ADVANCED_FACE('',(#2248),#965,.T.);
#15792=ADVANCED_FACE('',(#2249),#966,.T.);
#15793=ADVANCED_FACE('',(#2250),#967,.T.);
#15794=ADVANCED_FACE('',(#2251),#968,.T.);
#15795=ADVANCED_FACE('',(#2252),#969,.T.);
#15796=ADVANCED_FACE('',(#2253),#970,.T.);
#15797=ADVANCED_FACE('',(#2254),#971,.T.);
#15798=ADVANCED_FACE('',(#2255),#972,.T.);
#15799=ADVANCED_FACE('',(#2256),#973,.T.);
#15800=ADVANCED_FACE('',(#2257),#974,.T.);
#15801=ADVANCED_FACE('',(#2258),#975,.T.);
#15802=ADVANCED_FACE('',(#2259),#976,.T.);
#15803=ADVANCED_FACE('',(#2260),#977,.T.);
#15804=ADVANCED_FACE('',(#2261),#978,.T.);
#15805=ADVANCED_FACE('',(#2262),#979,.T.);
#15806=ADVANCED_FACE('',(#2263),#980,.T.);
#15807=ADVANCED_FACE('',(#2264),#981,.T.);
#15808=ADVANCED_FACE('',(#2265),#982,.T.);
#15809=ADVANCED_FACE('',(#2266),#983,.T.);
#15810=ADVANCED_FACE('',(#2267),#984,.T.);
#15811=ADVANCED_FACE('',(#2268),#985,.T.);
#15812=ADVANCED_FACE('',(#2269),#986,.T.);
#15813=ADVANCED_FACE('',(#2270),#987,.T.);
#15814=ADVANCED_FACE('',(#2271),#988,.T.);
#15815=ADVANCED_FACE('',(#2272),#989,.T.);
#15816=ADVANCED_FACE('',(#2273),#990,.T.);
#15817=ADVANCED_FACE('',(#2274),#991,.T.);
#15818=ADVANCED_FACE('',(#2275),#992,.T.);
#15819=ADVANCED_FACE('',(#2276),#993,.T.);
#15820=ADVANCED_FACE('',(#2277),#994,.T.);
#15821=ADVANCED_FACE('',(#2278),#995,.T.);
#15822=ADVANCED_FACE('',(#2279),#15086,.F.);
#15823=ADVANCED_FACE('',(#2280),#15087,.F.);
#15824=ADVANCED_FACE('',(#2281),#15088,.F.);
#15825=ADVANCED_FACE('',(#2282),#15089,.F.);
#15826=ADVANCED_FACE('',(#2283),#15090,.F.);
#15827=ADVANCED_FACE('',(#2284),#996,.F.);
#15828=ADVANCED_FACE('',(#2285),#15091,.F.);
#15829=ADVANCED_FACE('',(#2286),#503,.F.);
#15830=ADVANCED_FACE('',(#2287),#15092,.T.);
#15831=ADVANCED_FACE('',(#2288),#997,.T.);
#15832=ADVANCED_FACE('',(#2289),#504,.F.);
#15833=ADVANCED_FACE('',(#2290),#15093,.F.);
#15834=ADVANCED_FACE('',(#2291),#15094,.F.);
#15835=ADVANCED_FACE('',(#2292),#15095,.F.);
#15836=ADVANCED_FACE('',(#2293),#15096,.F.);
#15837=ADVANCED_FACE('',(#2294),#15097,.F.);
#15838=ADVANCED_FACE('',(#2295),#15098,.F.);
#15839=ADVANCED_FACE('',(#2296),#15099,.F.);
#15840=ADVANCED_FACE('',(#2297),#15100,.F.);
#15841=ADVANCED_FACE('',(#2298),#15101,.F.);
#15842=ADVANCED_FACE('',(#2299),#15102,.F.);
#15843=ADVANCED_FACE('',(#2300),#15103,.F.);
#15844=ADVANCED_FACE('',(#2301),#15104,.F.);
#15845=ADVANCED_FACE('',(#2302),#15105,.F.);
#15846=ADVANCED_FACE('',(#2303),#15106,.F.);
#15847=ADVANCED_FACE('',(#2304),#15107,.F.);
#15848=ADVANCED_FACE('',(#2305),#15108,.F.);
#15849=ADVANCED_FACE('',(#2306),#15109,.F.);
#15850=ADVANCED_FACE('',(#2307),#15110,.F.);
#15851=ADVANCED_FACE('',(#2308),#15111,.F.);
#15852=ADVANCED_FACE('',(#2309),#15112,.F.);
#15853=ADVANCED_FACE('',(#2310),#15113,.F.);
#15854=ADVANCED_FACE('',(#2311),#15114,.F.);
#15855=ADVANCED_FACE('',(#2312),#15115,.F.);
#15856=ADVANCED_FACE('',(#2313),#15116,.F.);
#15857=ADVANCED_FACE('',(#2314),#15117,.F.);
#15858=ADVANCED_FACE('',(#2315),#15118,.F.);
#15859=ADVANCED_FACE('',(#2316),#15119,.F.);
#15860=ADVANCED_FACE('',(#2317),#15120,.F.);
#15861=ADVANCED_FACE('',(#2318),#15121,.F.);
#15862=ADVANCED_FACE('',(#2319),#15122,.F.);
#15863=ADVANCED_FACE('',(#2320),#15123,.F.);
#15864=ADVANCED_FACE('',(#2321),#15124,.F.);
#15865=ADVANCED_FACE('',(#2322),#15125,.F.);
#15866=ADVANCED_FACE('',(#2323),#15126,.F.);
#15867=ADVANCED_FACE('',(#2324),#15127,.F.);
#15868=ADVANCED_FACE('',(#2325),#15128,.F.);
#15869=ADVANCED_FACE('',(#2326),#15129,.F.);
#15870=ADVANCED_FACE('',(#2327),#15130,.F.);
#15871=ADVANCED_FACE('',(#2328),#15131,.F.);
#15872=ADVANCED_FACE('',(#2329),#15132,.F.);
#15873=ADVANCED_FACE('',(#2330),#15133,.F.);
#15874=ADVANCED_FACE('',(#2331),#15134,.F.);
#15875=ADVANCED_FACE('',(#2332),#15135,.F.);
#15876=ADVANCED_FACE('',(#2333),#15136,.F.);
#15877=ADVANCED_FACE('',(#2334),#15137,.F.);
#15878=ADVANCED_FACE('',(#2335),#15138,.F.);
#15879=ADVANCED_FACE('',(#2336),#15139,.F.);
#15880=ADVANCED_FACE('',(#2337),#15140,.F.);
#15881=ADVANCED_FACE('',(#2338),#15141,.F.);
#15882=ADVANCED_FACE('',(#2339),#15142,.F.);
#15883=ADVANCED_FACE('',(#2340),#15143,.F.);
#15884=ADVANCED_FACE('',(#2341),#15144,.F.);
#15885=ADVANCED_FACE('',(#2342),#15145,.F.);
#15886=ADVANCED_FACE('',(#2343),#15146,.F.);
#15887=ADVANCED_FACE('',(#2344),#15147,.F.);
#15888=ADVANCED_FACE('',(#2345),#15148,.F.);
#15889=ADVANCED_FACE('',(#2346),#15149,.F.);
#15890=ADVANCED_FACE('',(#2347),#15150,.F.);
#15891=ADVANCED_FACE('',(#2348),#15151,.F.);
#15892=ADVANCED_FACE('',(#2349),#15152,.F.);
#15893=ADVANCED_FACE('',(#2350),#998,.T.);
#15894=ADVANCED_FACE('',(#2351),#999,.T.);
#15895=ADVANCED_FACE('',(#2352),#1000,.T.);
#15896=ADVANCED_FACE('',(#2353),#1001,.T.);
#15897=ADVANCED_FACE('',(#2354),#1002,.T.);
#15898=ADVANCED_FACE('',(#2355),#1003,.T.);
#15899=ADVANCED_FACE('',(#2356),#1004,.T.);
#15900=ADVANCED_FACE('',(#2357),#1005,.T.);
#15901=ADVANCED_FACE('',(#2358),#1006,.T.);
#15902=ADVANCED_FACE('',(#2359),#1007,.T.);
#15903=ADVANCED_FACE('',(#2360),#1008,.T.);
#15904=ADVANCED_FACE('',(#2361),#1009,.T.);
#15905=ADVANCED_FACE('',(#2362),#1010,.T.);
#15906=ADVANCED_FACE('',(#2363),#1011,.T.);
#15907=ADVANCED_FACE('',(#2364),#1012,.T.);
#15908=ADVANCED_FACE('',(#2365),#1013,.T.);
#15909=ADVANCED_FACE('',(#2366),#1014,.T.);
#15910=ADVANCED_FACE('',(#2367),#1015,.T.);
#15911=ADVANCED_FACE('',(#2368),#1016,.T.);
#15912=ADVANCED_FACE('',(#2369),#1017,.T.);
#15913=ADVANCED_FACE('',(#2370),#1018,.T.);
#15914=ADVANCED_FACE('',(#2371),#1019,.T.);
#15915=ADVANCED_FACE('',(#2372),#1020,.T.);
#15916=ADVANCED_FACE('',(#2373),#1021,.T.);
#15917=ADVANCED_FACE('',(#2374),#1022,.T.);
#15918=ADVANCED_FACE('',(#2375),#1023,.T.);
#15919=ADVANCED_FACE('',(#2376),#1024,.T.);
#15920=ADVANCED_FACE('',(#2377),#1025,.T.);
#15921=ADVANCED_FACE('',(#2378),#1026,.T.);
#15922=ADVANCED_FACE('',(#2379),#1027,.T.);
#15923=ADVANCED_FACE('',(#2380),#1765,.T.);
#15924=ADVANCED_FACE('',(#2381,#1199),#15153,.T.);
#15925=ADVANCED_FACE('',(#2382),#1766,.T.);
#15926=ADVANCED_FACE('',(#2383),#1028,.T.);
#15927=ADVANCED_FACE('',(#2384,#1200),#15154,.T.);
#15928=ADVANCED_FACE('',(#2385),#1767,.T.);
#15929=ADVANCED_FACE('',(#2386,#1201),#15155,.T.);
#15930=ADVANCED_FACE('',(#2387),#95,.T.);
#15931=ADVANCED_FACE('',(#2388),#505,.T.);
#15932=ADVANCED_FACE('',(#2389),#15156,.T.);
#15933=ADVANCED_FACE('',(#2390),#15157,.F.);
#15934=ADVANCED_FACE('',(#2391),#1029,.T.);
#15935=ADVANCED_FACE('',(#2392),#1030,.T.);
#15936=ADVANCED_FACE('',(#2393),#1031,.T.);
#15937=ADVANCED_FACE('',(#2394),#1032,.T.);
#15938=ADVANCED_FACE('',(#2395),#1033,.T.);
#15939=ADVANCED_FACE('',(#2396),#1034,.T.);
#15940=ADVANCED_FACE('',(#2397),#1035,.T.);
#15941=ADVANCED_FACE('',(#2398),#1036,.T.);
#15942=ADVANCED_FACE('',(#2399),#1037,.T.);
#15943=ADVANCED_FACE('',(#2400),#1038,.T.);
#15944=ADVANCED_FACE('',(#2401),#1039,.T.);
#15945=ADVANCED_FACE('',(#2402),#1040,.T.);
#15946=ADVANCED_FACE('',(#2403),#1041,.T.);
#15947=ADVANCED_FACE('',(#2404),#1042,.T.);
#15948=ADVANCED_FACE('',(#2405),#1043,.T.);
#15949=ADVANCED_FACE('',(#2406),#1044,.T.);
#15950=ADVANCED_FACE('',(#2407),#1045,.T.);
#15951=ADVANCED_FACE('',(#2408),#1046,.T.);
#15952=ADVANCED_FACE('',(#2409),#1047,.T.);
#15953=ADVANCED_FACE('',(#2410),#1048,.T.);
#15954=ADVANCED_FACE('',(#2411),#1049,.T.);
#15955=ADVANCED_FACE('',(#2412),#1050,.T.);
#15956=ADVANCED_FACE('',(#2413),#1051,.T.);
#15957=ADVANCED_FACE('',(#2414),#1052,.T.);
#15958=ADVANCED_FACE('',(#2415),#1053,.T.);
#15959=ADVANCED_FACE('',(#2416),#1054,.T.);
#15960=ADVANCED_FACE('',(#2417),#1055,.T.);
#15961=ADVANCED_FACE('',(#2418),#1056,.T.);
#15962=ADVANCED_FACE('',(#2419),#1057,.T.);
#15963=ADVANCED_FACE('',(#2420),#1058,.T.);
#15964=ADVANCED_FACE('',(#2421),#1059,.T.);
#15965=ADVANCED_FACE('',(#2422),#1060,.T.);
#15966=ADVANCED_FACE('',(#2423),#1061,.T.);
#15967=ADVANCED_FACE('',(#2424),#1062,.T.);
#15968=ADVANCED_FACE('',(#2425),#1063,.T.);
#15969=ADVANCED_FACE('',(#2426),#1064,.T.);
#15970=ADVANCED_FACE('',(#2427),#1065,.T.);
#15971=ADVANCED_FACE('',(#2428),#1066,.T.);
#15972=ADVANCED_FACE('',(#2429),#1067,.T.);
#15973=ADVANCED_FACE('',(#2430),#1068,.T.);
#15974=ADVANCED_FACE('',(#2431),#1069,.T.);
#15975=ADVANCED_FACE('',(#2432),#1070,.T.);
#15976=ADVANCED_FACE('',(#2433),#1071,.T.);
#15977=ADVANCED_FACE('',(#2434),#1072,.T.);
#15978=ADVANCED_FACE('',(#2435),#15158,.F.);
#15979=ADVANCED_FACE('',(#2436),#506,.F.);
#15980=ADVANCED_FACE('',(#2437),#15159,.T.);
#15981=ADVANCED_FACE('',(#2438),#1073,.T.);
#15982=ADVANCED_FACE('',(#2439),#507,.F.);
#15983=ADVANCED_FACE('',(#2440),#489,.F.);
#15984=ADVANCED_FACE('',(#2441),#1074,.T.);
#15985=ADVANCED_FACE('',(#2442,#1202),#15160,.T.);
#15986=ADVANCED_FACE('',(#2443),#15161,.F.);
#15987=ADVANCED_FACE('',(#2444),#15162,.F.);
#15988=ADVANCED_FACE('',(#2445),#15163,.F.);
#15989=ADVANCED_FACE('',(#2446),#15164,.F.);
#15990=ADVANCED_FACE('',(#2447),#15165,.F.);
#15991=ADVANCED_FACE('',(#2448),#15166,.F.);
#15992=ADVANCED_FACE('',(#2449),#1768,.F.);
#15993=ADVANCED_FACE('',(#2450),#15167,.F.);
#15994=ADVANCED_FACE('',(#2451),#15168,.F.);
#15995=ADVANCED_FACE('',(#2452),#15169,.F.);
#15996=ADVANCED_FACE('',(#2453),#15170,.F.);
#15997=ADVANCED_FACE('',(#2454),#15171,.F.);
#15998=ADVANCED_FACE('',(#2455),#15172,.F.);
#15999=ADVANCED_FACE('',(#2456),#15173,.F.);
#16000=ADVANCED_FACE('',(#2457),#15174,.F.);
#16001=ADVANCED_FACE('',(#2458),#15175,.F.);
#16002=ADVANCED_FACE('',(#2459),#15176,.F.);
#16003=ADVANCED_FACE('',(#2460),#15177,.F.);
#16004=ADVANCED_FACE('',(#2461),#15178,.F.);
#16005=ADVANCED_FACE('',(#2462),#15179,.F.);
#16006=ADVANCED_FACE('',(#2463),#15180,.F.);
#16007=ADVANCED_FACE('',(#2464),#15181,.F.);
#16008=ADVANCED_FACE('',(#2465),#15182,.F.);
#16009=ADVANCED_FACE('',(#2466),#15183,.F.);
#16010=ADVANCED_FACE('',(#2467),#15184,.F.);
#16011=ADVANCED_FACE('',(#2468),#15185,.F.);
#16012=ADVANCED_FACE('',(#2469),#15186,.F.);
#16013=ADVANCED_FACE('',(#2470),#15187,.F.);
#16014=ADVANCED_FACE('',(#2471),#15188,.F.);
#16015=ADVANCED_FACE('',(#2472),#15189,.F.);
#16016=ADVANCED_FACE('',(#2473),#15190,.F.);
#16017=ADVANCED_FACE('',(#2474),#15191,.F.);
#16018=ADVANCED_FACE('',(#2475),#15192,.F.);
#16019=ADVANCED_FACE('',(#2476),#15193,.F.);
#16020=ADVANCED_FACE('',(#2477),#15194,.F.);
#16021=ADVANCED_FACE('',(#2478),#15195,.F.);
#16022=ADVANCED_FACE('',(#2479),#15196,.F.);
#16023=ADVANCED_FACE('',(#2480),#15197,.F.);
#16024=ADVANCED_FACE('',(#2481),#15198,.F.);
#16025=ADVANCED_FACE('',(#2482),#15199,.F.);
#16026=ADVANCED_FACE('',(#2483),#15200,.F.);
#16027=ADVANCED_FACE('',(#2484),#15201,.F.);
#16028=ADVANCED_FACE('',(#2485),#15202,.F.);
#16029=ADVANCED_FACE('',(#2486),#15203,.F.);
#16030=ADVANCED_FACE('',(#2487),#15204,.F.);
#16031=ADVANCED_FACE('',(#2488),#15205,.F.);
#16032=ADVANCED_FACE('',(#2489),#15206,.F.);
#16033=ADVANCED_FACE('',(#2490),#15207,.F.);
#16034=ADVANCED_FACE('',(#2491),#15208,.F.);
#16035=ADVANCED_FACE('',(#2492),#15209,.F.);
#16036=ADVANCED_FACE('',(#2493),#15210,.F.);
#16037=ADVANCED_FACE('',(#2494),#15211,.F.);
#16038=ADVANCED_FACE('',(#2495),#15212,.F.);
#16039=ADVANCED_FACE('',(#2496),#15213,.F.);
#16040=ADVANCED_FACE('',(#2497),#15214,.F.);
#16041=ADVANCED_FACE('',(#2498),#15215,.F.);
#16042=ADVANCED_FACE('',(#2499),#15216,.F.);
#16043=ADVANCED_FACE('',(#2500),#15217,.F.);
#16044=ADVANCED_FACE('',(#2501),#15218,.F.);
#16045=ADVANCED_FACE('',(#2502),#15219,.F.);
#16046=ADVANCED_FACE('',(#2503),#15220,.F.);
#16047=ADVANCED_FACE('',(#2504),#15221,.F.);
#16048=ADVANCED_FACE('',(#2505),#15222,.F.);
#16049=ADVANCED_FACE('',(#2506),#15223,.F.);
#16050=ADVANCED_FACE('',(#2507),#15224,.F.);
#16051=ADVANCED_FACE('',(#2508),#15225,.F.);
#16052=ADVANCED_FACE('',(#2509),#15226,.F.);
#16053=ADVANCED_FACE('',(#2510),#15227,.F.);
#16054=ADVANCED_FACE('',(#2511),#15228,.F.);
#16055=ADVANCED_FACE('',(#2512),#15229,.F.);
#16056=ADVANCED_FACE('',(#2513),#15230,.F.);
#16057=ADVANCED_FACE('',(#2514),#15231,.F.);
#16058=ADVANCED_FACE('',(#2515),#15232,.F.);
#16059=ADVANCED_FACE('',(#2516),#15233,.F.);
#16060=ADVANCED_FACE('',(#2517),#15234,.F.);
#16061=ADVANCED_FACE('',(#2518),#15235,.F.);
#16062=ADVANCED_FACE('',(#2519),#15236,.F.);
#16063=ADVANCED_FACE('',(#2520),#15237,.F.);
#16064=ADVANCED_FACE('',(#2521),#15238,.F.);
#16065=ADVANCED_FACE('',(#2522),#15239,.F.);
#16066=ADVANCED_FACE('',(#2523),#15240,.F.);
#16067=ADVANCED_FACE('',(#2524),#15241,.F.);
#16068=ADVANCED_FACE('',(#2525),#15242,.F.);
#16069=ADVANCED_FACE('',(#2526),#15243,.F.);
#16070=ADVANCED_FACE('',(#2527),#15244,.F.);
#16071=ADVANCED_FACE('',(#2528),#15245,.F.);
#16072=ADVANCED_FACE('',(#2529),#15246,.F.);
#16073=ADVANCED_FACE('',(#2530),#15247,.F.);
#16074=ADVANCED_FACE('',(#2531),#15248,.F.);
#16075=ADVANCED_FACE('',(#2532),#15249,.F.);
#16076=ADVANCED_FACE('',(#2533),#15250,.F.);
#16077=ADVANCED_FACE('',(#2534),#15251,.F.);
#16078=ADVANCED_FACE('',(#2535),#15252,.F.);
#16079=ADVANCED_FACE('',(#2536),#15253,.F.);
#16080=ADVANCED_FACE('',(#2537),#15254,.F.);
#16081=ADVANCED_FACE('',(#2538),#15255,.F.);
#16082=ADVANCED_FACE('',(#2539),#15256,.F.);
#16083=ADVANCED_FACE('',(#2540),#15257,.F.);
#16084=ADVANCED_FACE('',(#2541),#15258,.F.);
#16085=ADVANCED_FACE('',(#2542),#15259,.F.);
#16086=ADVANCED_FACE('',(#2543),#15260,.F.);
#16087=ADVANCED_FACE('',(#2544),#15261,.F.);
#16088=ADVANCED_FACE('',(#2545),#15262,.F.);
#16089=ADVANCED_FACE('',(#2546),#1075,.T.);
#16090=ADVANCED_FACE('',(#2547),#1076,.T.);
#16091=ADVANCED_FACE('',(#2548),#1077,.T.);
#16092=ADVANCED_FACE('',(#2549),#1078,.T.);
#16093=ADVANCED_FACE('',(#2550),#1079,.T.);
#16094=ADVANCED_FACE('',(#2551),#1080,.T.);
#16095=ADVANCED_FACE('',(#2552),#1081,.T.);
#16096=ADVANCED_FACE('',(#2553),#1082,.T.);
#16097=ADVANCED_FACE('',(#2554),#1083,.T.);
#16098=ADVANCED_FACE('',(#2555),#1084,.T.);
#16099=ADVANCED_FACE('',(#2556),#1085,.T.);
#16100=ADVANCED_FACE('',(#2557),#1086,.T.);
#16101=ADVANCED_FACE('',(#2558),#1087,.T.);
#16102=ADVANCED_FACE('',(#2559),#1088,.T.);
#16103=ADVANCED_FACE('',(#2560),#1089,.T.);
#16104=ADVANCED_FACE('',(#2561),#1090,.T.);
#16105=ADVANCED_FACE('',(#2562),#1091,.T.);
#16106=ADVANCED_FACE('',(#2563),#1092,.T.);
#16107=ADVANCED_FACE('',(#2564),#1093,.T.);
#16108=ADVANCED_FACE('',(#2565),#1094,.T.);
#16109=ADVANCED_FACE('',(#2566),#1095,.T.);
#16110=ADVANCED_FACE('',(#2567),#1096,.T.);
#16111=ADVANCED_FACE('',(#2568),#1097,.T.);
#16112=ADVANCED_FACE('',(#2569),#1098,.T.);
#16113=ADVANCED_FACE('',(#2570),#1099,.T.);
#16114=ADVANCED_FACE('',(#2571),#1100,.T.);
#16115=ADVANCED_FACE('',(#2572),#1101,.T.);
#16116=ADVANCED_FACE('',(#2573),#1102,.T.);
#16117=ADVANCED_FACE('',(#2574),#1103,.T.);
#16118=ADVANCED_FACE('',(#2575),#1104,.T.);
#16119=ADVANCED_FACE('',(#2576),#1105,.T.);
#16120=ADVANCED_FACE('',(#2577),#1106,.T.);
#16121=ADVANCED_FACE('',(#2578),#1107,.T.);
#16122=ADVANCED_FACE('',(#2579),#1108,.T.);
#16123=ADVANCED_FACE('',(#2580),#1109,.T.);
#16124=ADVANCED_FACE('',(#2581),#1110,.T.);
#16125=ADVANCED_FACE('',(#2582),#15263,.T.);
#16126=ADVANCED_FACE('',(#2583),#1769,.T.);
#16127=ADVANCED_FACE('',(#2584),#1770,.T.);
#16128=ADVANCED_FACE('',(#2585,#1203),#15264,.T.);
#16129=ADVANCED_FACE('',(#2586),#1111,.T.);
#16130=ADVANCED_FACE('',(#2587),#1112,.T.);
#16131=ADVANCED_FACE('',(#2588),#1113,.T.);
#16132=ADVANCED_FACE('',(#2589),#1114,.T.);
#16133=ADVANCED_FACE('',(#2590),#1115,.T.);
#16134=ADVANCED_FACE('',(#2591),#1116,.T.);
#16135=ADVANCED_FACE('',(#2592),#1117,.T.);
#16136=ADVANCED_FACE('',(#2593),#1118,.T.);
#16137=ADVANCED_FACE('',(#2594),#1119,.T.);
#16138=ADVANCED_FACE('',(#2595),#1120,.T.);
#16139=ADVANCED_FACE('',(#2596),#1121,.T.);
#16140=ADVANCED_FACE('',(#2597),#1122,.T.);
#16141=ADVANCED_FACE('',(#2598),#1123,.T.);
#16142=ADVANCED_FACE('',(#2599),#1124,.T.);
#16143=ADVANCED_FACE('',(#2600),#1125,.T.);
#16144=ADVANCED_FACE('',(#2601),#1126,.T.);
#16145=ADVANCED_FACE('',(#2602),#1127,.T.);
#16146=ADVANCED_FACE('',(#2603),#1128,.T.);
#16147=ADVANCED_FACE('',(#2604),#1129,.T.);
#16148=ADVANCED_FACE('',(#2605),#1130,.T.);
#16149=ADVANCED_FACE('',(#2606),#1131,.T.);
#16150=ADVANCED_FACE('',(#2607),#1132,.T.);
#16151=ADVANCED_FACE('',(#2608),#508,.F.);
#16152=ADVANCED_FACE('',(#2609),#15265,.T.);
#16153=ADVANCED_FACE('',(#2610),#1133,.T.);
#16154=ADVANCED_FACE('',(#2611),#509,.F.);
#16155=ADVANCED_FACE('',(#2612),#15266,.F.);
#16156=ADVANCED_FACE('',(#2613),#15267,.F.);
#16157=ADVANCED_FACE('',(#2614),#15268,.F.);
#16158=ADVANCED_FACE('',(#2615),#15269,.F.);
#16159=ADVANCED_FACE('',(#2616),#15270,.F.);
#16160=ADVANCED_FACE('',(#2617),#15271,.F.);
#16161=ADVANCED_FACE('',(#2618),#15272,.F.);
#16162=ADVANCED_FACE('',(#2619),#15273,.F.);
#16163=ADVANCED_FACE('',(#2620),#15274,.F.);
#16164=ADVANCED_FACE('',(#2621),#15275,.F.);
#16165=ADVANCED_FACE('',(#2622),#15276,.F.);
#16166=ADVANCED_FACE('',(#2623),#15277,.F.);
#16167=ADVANCED_FACE('',(#2624),#15278,.F.);
#16168=ADVANCED_FACE('',(#2625),#15279,.F.);
#16169=ADVANCED_FACE('',(#2626),#15280,.F.);
#16170=ADVANCED_FACE('',(#2627),#15281,.F.);
#16171=ADVANCED_FACE('',(#2628),#15282,.F.);
#16172=ADVANCED_FACE('',(#2629),#15283,.F.);
#16173=ADVANCED_FACE('',(#2630),#15284,.F.);
#16174=ADVANCED_FACE('',(#2631),#15285,.F.);
#16175=ADVANCED_FACE('',(#2632),#15286,.F.);
#16176=ADVANCED_FACE('',(#2633),#15287,.F.);
#16177=ADVANCED_FACE('',(#2634),#15288,.F.);
#16178=ADVANCED_FACE('',(#2635),#15289,.F.);
#16179=ADVANCED_FACE('',(#2636),#15290,.F.);
#16180=ADVANCED_FACE('',(#2637),#15291,.F.);
#16181=ADVANCED_FACE('',(#2638),#15292,.F.);
#16182=ADVANCED_FACE('',(#2639),#15293,.F.);
#16183=ADVANCED_FACE('',(#2640),#15294,.F.);
#16184=ADVANCED_FACE('',(#2641),#15295,.F.);
#16185=ADVANCED_FACE('',(#2642),#15296,.F.);
#16186=ADVANCED_FACE('',(#2643),#15297,.F.);
#16187=ADVANCED_FACE('',(#2644),#15298,.F.);
#16188=ADVANCED_FACE('',(#2645),#15299,.F.);
#16189=ADVANCED_FACE('',(#2646),#15300,.F.);
#16190=ADVANCED_FACE('',(#2647),#15301,.F.);
#16191=ADVANCED_FACE('',(#2648),#15302,.F.);
#16192=ADVANCED_FACE('',(#2649),#15303,.F.);
#16193=ADVANCED_FACE('',(#2650),#15304,.F.);
#16194=ADVANCED_FACE('',(#2651),#15305,.F.);
#16195=ADVANCED_FACE('',(#2652),#15306,.F.);
#16196=ADVANCED_FACE('',(#2653),#15307,.F.);
#16197=ADVANCED_FACE('',(#2654),#15308,.F.);
#16198=ADVANCED_FACE('',(#2655),#15309,.F.);
#16199=ADVANCED_FACE('',(#2656),#15310,.F.);
#16200=ADVANCED_FACE('',(#2657),#15311,.F.);
#16201=ADVANCED_FACE('',(#2658),#15312,.F.);
#16202=ADVANCED_FACE('',(#2659),#15313,.F.);
#16203=ADVANCED_FACE('',(#2660),#1134,.T.);
#16204=ADVANCED_FACE('',(#2661),#1135,.T.);
#16205=ADVANCED_FACE('',(#2662),#1136,.T.);
#16206=ADVANCED_FACE('',(#2663),#1137,.T.);
#16207=ADVANCED_FACE('',(#2664),#1138,.T.);
#16208=ADVANCED_FACE('',(#2665),#1139,.T.);
#16209=ADVANCED_FACE('',(#2666),#1140,.T.);
#16210=ADVANCED_FACE('',(#2667),#1141,.T.);
#16211=ADVANCED_FACE('',(#2668),#1142,.T.);
#16212=ADVANCED_FACE('',(#2669),#1143,.T.);
#16213=ADVANCED_FACE('',(#2670),#1144,.T.);
#16214=ADVANCED_FACE('',(#2671),#1145,.T.);
#16215=ADVANCED_FACE('',(#2672),#1146,.T.);
#16216=ADVANCED_FACE('',(#2673),#1147,.T.);
#16217=ADVANCED_FACE('',(#2674),#1148,.T.);
#16218=ADVANCED_FACE('',(#2675),#1149,.T.);
#16219=ADVANCED_FACE('',(#2676),#1150,.T.);
#16220=ADVANCED_FACE('',(#2677),#1151,.T.);
#16221=ADVANCED_FACE('',(#2678),#1152,.T.);
#16222=ADVANCED_FACE('',(#2679),#1153,.T.);
#16223=ADVANCED_FACE('',(#2680),#1154,.T.);
#16224=ADVANCED_FACE('',(#2681),#1155,.T.);
#16225=ADVANCED_FACE('',(#2682),#1156,.T.);
#16226=ADVANCED_FACE('',(#2683),#1157,.T.);
#16227=ADVANCED_FACE('',(#2684),#1771,.T.);
#16228=ADVANCED_FACE('',(#2685),#15314,.T.);
#16229=ADVANCED_FACE('',(#2686),#1772,.T.);
#16230=ADVANCED_FACE('',(#2687),#1158,.T.);
#16231=ADVANCED_FACE('',(#2688,#1204),#15315,.T.);
#16232=ADVANCED_FACE('',(#2689),#1773,.T.);
#16233=ADVANCED_FACE('',(#2690),#15316,.T.);
#16234=CLOSED_SHELL('',(#15317,#15318,#15319,#15320,#15321,#15322,#15323,
#15324,#15325,#15326,#15327,#15328,#15329,#15330,#15331,#15332,#15333,#15334,
#15335,#15336,#15337,#15338,#15339,#15340,#15341,#15342,#15343,#15344,#15345,
#15346,#15347,#15348,#15349,#15350,#15351,#15352,#15353,#15354,#15355,#15356,
#15357,#15358,#15359,#15360,#15361,#15362,#15363,#15364,#15365,#15366,#15367,
#15368,#15369,#15370,#15371,#15372,#15373,#15374,#15375,#15376,#15377,#15378,
#15379,#15380,#15381,#15382,#15383,#15384,#15385,#15386,#15387,#15388,#15389,
#15390,#15391,#15392,#15393,#15394,#15395,#15396,#15397,#15398,#15399,#15400,
#15401,#15402,#15403,#15404,#15405,#15406,#15407,#15408,#15409,#15410,#15411,
#15412,#15413,#15414,#15415,#15416,#15417,#15418,#15419,#15420,#15421,#15422,
#15423,#15424,#15425,#15426,#15427,#15428,#15429,#15430,#15431,#15432,#15433,
#15434,#15435,#15436,#15437,#15438,#15439,#15440));
#16235=CLOSED_SHELL('',(#15441,#15442,#15443,#15444,#15445,#15446,#15447,
#15448,#15449,#15450,#15451,#15452,#15453,#15454,#15455,#15456,#15457,#15458,
#15459,#15460,#15461,#15462,#15463));
#16236=CLOSED_SHELL('',(#15464,#15465,#15466,#15467,#15468,#15469,#15470,
#15471,#15472));
#16237=CLOSED_SHELL('',(#15473,#15474,#15475,#15476,#15477,#15478,#15479,
#15480,#15481,#15482,#15483,#15484,#15485,#15486,#15487,#15488,#15489,#15490,
#15491,#15492,#15493,#15494,#15495,#15496,#15497,#15498,#15499,#15500,#15501,
#15502,#15503,#15504,#15505,#15506,#15507,#15508,#15509,#15510,#15511,#15512,
#15513,#15514,#15515,#15516,#15517,#15518,#15519,#15520,#15521,#15522,#15523,
#15524,#15525,#15526,#15527,#15528,#15529,#15530,#15531,#15532,#15533,#15534,
#15535,#15536,#15537,#15538,#15539,#15540,#15541,#15542,#15543,#15544,#15545,
#15546,#15547,#15548,#15549,#15550,#15551,#15552));
#16238=CLOSED_SHELL('',(#15553,#15554,#15555,#15556,#15557));
#16239=CLOSED_SHELL('',(#15558,#15559,#15560,#15561,#15562,#15563,#15564,
#15565,#15566,#15567,#15568,#15569,#15570,#15571,#15572,#15573,#15574,#15575,
#15576,#15577,#15578,#15579,#15580,#15581,#15582,#15583,#15584,#15585,#15586,
#15587,#15588,#15589));
#16240=CLOSED_SHELL('',(#15590,#15591,#15592,#15593,#15594,#15595,#15596,
#15597,#15598,#15599,#15600,#15601,#15602,#15603,#15604,#15605,#15606,#15607,
#15608,#15609,#15610,#15611,#15612,#15613,#15614,#15615,#15616,#15617,#15618,
#15619,#15620,#15621,#15622,#15623,#15624,#15625,#15626,#15627,#15628,#15629,
#15630,#15631,#15632,#15633,#15634,#15635,#15636,#15637,#15638,#15639,#15640,
#15641,#15642));
#16241=CLOSED_SHELL('',(#15643,#15644,#15645,#15646,#15647,#15648,#15649,
#15650,#15651,#15652,#15653,#15654,#15655,#15656,#15657,#15658,#15659,#15660,
#15661,#15662,#15663,#15664,#15665,#15666,#15667,#15668,#15669,#15670,#15671,
#15672,#15673,#15674,#15675,#15676,#15677,#15678,#15679,#15680,#15681,#15682,
#15683,#15684,#15685,#15686,#15687,#15688,#15689,#15690,#15691,#15692,#15693));
#16242=CLOSED_SHELL('',(#15694,#15695,#15696,#15697,#15698,#15699,#15700,
#15701,#15702,#15703,#15704,#15705,#15706,#15707,#15708,#15709,#15710,#15711,
#15712,#15713,#15714,#15715,#15716,#15717,#15718,#15719,#15720,#15721,#15722,
#15723,#15724,#15725,#15726,#15727,#15728,#15729,#15730,#15731,#15732,#15733,
#15734,#15735,#15736,#15737,#15738,#15739,#15740,#15741,#15742,#15743,#15744,
#15745,#15746,#15747,#15748,#15749,#15750,#15751,#15752,#15753,#15754,#15755,
#15756,#15757,#15758,#15759,#15760,#15761,#15762,#15763,#15764,#15765,#15766,
#15767,#15768,#15769,#15770,#15771,#15772,#15773,#15774));
#16243=CLOSED_SHELL('',(#15775,#15776,#15777,#15778,#15779,#15780,#15781,
#15782,#15783,#15784,#15785,#15786,#15787,#15788,#15789,#15790,#15791,#15792,
#15793,#15794,#15795,#15796,#15797,#15798,#15799,#15800,#15801,#15802,#15803,
#15804,#15805,#15806,#15807,#15808,#15809,#15810,#15811,#15812,#15813,#15814,
#15815,#15816,#15817,#15818,#15819,#15820,#15821,#15822,#15823,#15824,#15825,
#15826,#15827,#15828,#15829,#15830,#15831,#15832,#15833,#15834,#15835,#15836,
#15837,#15838,#15839,#15840,#15841,#15842,#15843,#15844,#15845,#15846,#15847,
#15848,#15849,#15850,#15851,#15852,#15853,#15854,#15855,#15856,#15857,#15858,
#15859,#15860,#15861,#15862,#15863,#15864,#15865,#15866,#15867,#15868,#15869,
#15870,#15871,#15872,#15873,#15874,#15875,#15876,#15877,#15878,#15879,#15880,
#15881,#15882,#15883,#15884,#15885,#15886,#15887,#15888,#15889,#15890,#15891,
#15892,#15893,#15894,#15895,#15896,#15897,#15898,#15899,#15900,#15901,#15902,
#15903,#15904,#15905,#15906,#15907,#15908,#15909,#15910,#15911,#15912,#15913,
#15914,#15915,#15916,#15917,#15918,#15919,#15920,#15921,#15922,#15923,#15924,
#15925,#15926,#15927,#15928,#15929));
#16244=CLOSED_SHELL('',(#15930));
#16245=CLOSED_SHELL('',(#15931,#15932,#15933));
#16246=CLOSED_SHELL('',(#15934,#15935,#15936,#15937,#15938,#15939,#15940,
#15941,#15942,#15943,#15944,#15945,#15946,#15947,#15948,#15949,#15950,#15951,
#15952,#15953,#15954,#15955,#15956,#15957,#15958,#15959,#15960,#15961,#15962,
#15963,#15964,#15965,#15966,#15967,#15968,#15969,#15970,#15971,#15972,#15973,
#15974,#15975,#15976,#15977,#15978,#15979,#15980,#15981,#15982,#15983,#15984,
#15985,#15986,#15987,#15988,#15989,#15990,#15991,#15992,#15993,#15994,#15995,
#15996,#15997,#15998,#15999,#16000,#16001,#16002,#16003,#16004,#16005,#16006,
#16007,#16008,#16009,#16010,#16011,#16012,#16013,#16014,#16015,#16016,#16017,
#16018,#16019,#16020,#16021,#16022,#16023,#16024,#16025,#16026,#16027,#16028,
#16029,#16030,#16031,#16032,#16033,#16034,#16035,#16036,#16037,#16038,#16039,
#16040,#16041,#16042,#16043,#16044,#16045,#16046,#16047,#16048,#16049,#16050,
#16051,#16052,#16053,#16054,#16055,#16056,#16057,#16058,#16059,#16060,#16061,
#16062,#16063,#16064,#16065,#16066,#16067,#16068,#16069,#16070,#16071,#16072,
#16073,#16074,#16075,#16076,#16077,#16078,#16079,#16080,#16081,#16082,#16083,
#16084,#16085,#16086,#16087,#16088,#16089,#16090,#16091,#16092,#16093,#16094,
#16095,#16096,#16097,#16098,#16099,#16100,#16101,#16102,#16103,#16104,#16105,
#16106,#16107,#16108,#16109,#16110,#16111,#16112,#16113,#16114,#16115,#16116,
#16117,#16118,#16119,#16120,#16121,#16122,#16123,#16124,#16125,#16126,#16127,
#16128));
#16247=CLOSED_SHELL('',(#16129,#16130,#16131,#16132,#16133,#16134,#16135,
#16136,#16137,#16138,#16139,#16140,#16141,#16142,#16143,#16144,#16145,#16146,
#16147,#16148,#16149,#16150,#16151,#16152,#16153,#16154,#16155,#16156,#16157,
#16158,#16159,#16160,#16161,#16162,#16163,#16164,#16165,#16166,#16167,#16168,
#16169,#16170,#16171,#16172,#16173,#16174,#16175,#16176,#16177,#16178,#16179,
#16180,#16181,#16182,#16183,#16184,#16185,#16186,#16187,#16188,#16189,#16190,
#16191,#16192,#16193,#16194,#16195,#16196,#16197,#16198,#16199,#16200,#16201,
#16202,#16203,#16204,#16205,#16206,#16207,#16208,#16209,#16210,#16211,#16212,
#16213,#16214,#16215,#16216,#16217,#16218,#16219,#16220,#16221,#16222,#16223,
#16224,#16225,#16226,#16227,#16228,#16229,#16230,#16231,#16232,#16233));
#16248=DERIVED_UNIT_ELEMENT(#16276,1.);
#16249=DERIVED_UNIT_ELEMENT(#38613,-3.);
#16250=DERIVED_UNIT_ELEMENT(#16276,1.);
#16251=DERIVED_UNIT_ELEMENT(#38613,-3.);
#16252=DERIVED_UNIT_ELEMENT(#16276,1.);
#16253=DERIVED_UNIT_ELEMENT(#38613,-3.);
#16254=DERIVED_UNIT_ELEMENT(#16276,1.);
#16255=DERIVED_UNIT_ELEMENT(#38613,-3.);
#16256=DERIVED_UNIT_ELEMENT(#16276,1.);
#16257=DERIVED_UNIT_ELEMENT(#38613,-3.);
#16258=DERIVED_UNIT_ELEMENT(#16276,1.);
#16259=DERIVED_UNIT_ELEMENT(#38613,-3.);
#16260=DERIVED_UNIT_ELEMENT(#16276,1.);
#16261=DERIVED_UNIT_ELEMENT(#38613,-3.);
#16262=DERIVED_UNIT_ELEMENT(#16276,1.);
#16263=DERIVED_UNIT_ELEMENT(#38613,-3.);
#16264=DERIVED_UNIT_ELEMENT(#16276,1.);
#16265=DERIVED_UNIT_ELEMENT(#38613,-3.);
#16266=DERIVED_UNIT_ELEMENT(#16276,1.);
#16267=DERIVED_UNIT_ELEMENT(#38613,-3.);
#16268=DERIVED_UNIT_ELEMENT(#16276,1.);
#16269=DERIVED_UNIT_ELEMENT(#38613,-3.);
#16270=DERIVED_UNIT_ELEMENT(#16276,1.);
#16271=DERIVED_UNIT_ELEMENT(#38613,-3.);
#16272=DERIVED_UNIT_ELEMENT(#16276,1.);
#16273=DERIVED_UNIT_ELEMENT(#38613,-3.);
#16274=DERIVED_UNIT_ELEMENT(#16276,1.);
#16275=DERIVED_UNIT_ELEMENT(#38613,-3.);
#16276=(
MASS_UNIT()
NAMED_UNIT(*)
SI_UNIT(.KILO.,.GRAM.)
);
#16277=DERIVED_UNIT((#16248,#16249));
#16278=DERIVED_UNIT((#16250,#16251));
#16279=DERIVED_UNIT((#16252,#16253));
#16280=DERIVED_UNIT((#16254,#16255));
#16281=DERIVED_UNIT((#16256,#16257));
#16282=DERIVED_UNIT((#16258,#16259));
#16283=DERIVED_UNIT((#16260,#16261));
#16284=DERIVED_UNIT((#16262,#16263));
#16285=DERIVED_UNIT((#16264,#16265));
#16286=DERIVED_UNIT((#16266,#16267));
#16287=DERIVED_UNIT((#16268,#16269));
#16288=DERIVED_UNIT((#16270,#16271));
#16289=DERIVED_UNIT((#16272,#16273));
#16290=DERIVED_UNIT((#16274,#16275));
#16291=MEASURE_REPRESENTATION_ITEM('density measure',
POSITIVE_RATIO_MEASURE(2700.),#16277);
#16292=MEASURE_REPRESENTATION_ITEM('density measure',
POSITIVE_RATIO_MEASURE(2700.),#16278);
#16293=MEASURE_REPRESENTATION_ITEM('density measure',
POSITIVE_RATIO_MEASURE(2700.),#16279);
#16294=MEASURE_REPRESENTATION_ITEM('density measure',
POSITIVE_RATIO_MEASURE(2700.),#16280);
#16295=MEASURE_REPRESENTATION_ITEM('density measure',
POSITIVE_RATIO_MEASURE(3180.),#16281);
#16296=MEASURE_REPRESENTATION_ITEM('density measure',
POSITIVE_RATIO_MEASURE(2700.),#16282);
#16297=MEASURE_REPRESENTATION_ITEM('density measure',
POSITIVE_RATIO_MEASURE(7850.),#16283);
#16298=MEASURE_REPRESENTATION_ITEM('density measure',
POSITIVE_RATIO_MEASURE(7850.),#16284);
#16299=MEASURE_REPRESENTATION_ITEM('density measure',
POSITIVE_RATIO_MEASURE(2700.),#16285);
#16300=MEASURE_REPRESENTATION_ITEM('density measure',
POSITIVE_RATIO_MEASURE(8490.),#16286);
#16301=MEASURE_REPRESENTATION_ITEM('density measure',
POSITIVE_RATIO_MEASURE(7850.),#16287);
#16302=MEASURE_REPRESENTATION_ITEM('density measure',
POSITIVE_RATIO_MEASURE(7850.),#16288);
#16303=MEASURE_REPRESENTATION_ITEM('density measure',
POSITIVE_RATIO_MEASURE(7850.),#16289);
#16304=MEASURE_REPRESENTATION_ITEM('density measure',
POSITIVE_RATIO_MEASURE(8490.),#16290);
#16305=PROPERTY_DEFINITION_REPRESENTATION(#16375,#16333);
#16306=PROPERTY_DEFINITION_REPRESENTATION(#16376,#16334);
#16307=PROPERTY_DEFINITION_REPRESENTATION(#16377,#16335);
#16308=PROPERTY_DEFINITION_REPRESENTATION(#16378,#16336);
#16309=PROPERTY_DEFINITION_REPRESENTATION(#16379,#16337);
#16310=PROPERTY_DEFINITION_REPRESENTATION(#16380,#16338);
#16311=PROPERTY_DEFINITION_REPRESENTATION(#16381,#16339);
#16312=PROPERTY_DEFINITION_REPRESENTATION(#16382,#16340);
#16313=PROPERTY_DEFINITION_REPRESENTATION(#16383,#16341);
#16314=PROPERTY_DEFINITION_REPRESENTATION(#16384,#16342);
#16315=PROPERTY_DEFINITION_REPRESENTATION(#16385,#16343);
#16316=PROPERTY_DEFINITION_REPRESENTATION(#16386,#16344);
#16317=PROPERTY_DEFINITION_REPRESENTATION(#16387,#16345);
#16318=PROPERTY_DEFINITION_REPRESENTATION(#16388,#16346);
#16319=PROPERTY_DEFINITION_REPRESENTATION(#16389,#16347);
#16320=PROPERTY_DEFINITION_REPRESENTATION(#16390,#16348);
#16321=PROPERTY_DEFINITION_REPRESENTATION(#16391,#16349);
#16322=PROPERTY_DEFINITION_REPRESENTATION(#16392,#16350);
#16323=PROPERTY_DEFINITION_REPRESENTATION(#16393,#16351);
#16324=PROPERTY_DEFINITION_REPRESENTATION(#16394,#16352);
#16325=PROPERTY_DEFINITION_REPRESENTATION(#16395,#16353);
#16326=PROPERTY_DEFINITION_REPRESENTATION(#16396,#16354);
#16327=PROPERTY_DEFINITION_REPRESENTATION(#16397,#16355);
#16328=PROPERTY_DEFINITION_REPRESENTATION(#16398,#16356);
#16329=PROPERTY_DEFINITION_REPRESENTATION(#16399,#16357);
#16330=PROPERTY_DEFINITION_REPRESENTATION(#16400,#16358);
#16331=PROPERTY_DEFINITION_REPRESENTATION(#16401,#16359);
#16332=PROPERTY_DEFINITION_REPRESENTATION(#16402,#16360);
#16333=REPRESENTATION('material name',(#16361),#38597);
#16334=REPRESENTATION('density',(#16291),#38597);
#16335=REPRESENTATION('material name',(#16362),#38598);
#16336=REPRESENTATION('density',(#16292),#38598);
#16337=REPRESENTATION('material name',(#16363),#38599);
#16338=REPRESENTATION('density',(#16293),#38599);
#16339=REPRESENTATION('material name',(#16364),#38600);
#16340=REPRESENTATION('density',(#16294),#38600);
#16341=REPRESENTATION('material name',(#16365),#38601);
#16342=REPRESENTATION('density',(#16295),#38601);
#16343=REPRESENTATION('material name',(#16366),#38602);
#16344=REPRESENTATION('density',(#16296),#38602);
#16345=REPRESENTATION('material name',(#16367),#38603);
#16346=REPRESENTATION('density',(#16297),#38603);
#16347=REPRESENTATION('material name',(#16368),#38604);
#16348=REPRESENTATION('density',(#16298),#38604);
#16349=REPRESENTATION('material name',(#16369),#38605);
#16350=REPRESENTATION('density',(#16299),#38605);
#16351=REPRESENTATION('material name',(#16370),#38606);
#16352=REPRESENTATION('density',(#16300),#38606);
#16353=REPRESENTATION('material name',(#16371),#38607);
#16354=REPRESENTATION('density',(#16301),#38607);
#16355=REPRESENTATION('material name',(#16372),#38608);
#16356=REPRESENTATION('density',(#16302),#38608);
#16357=REPRESENTATION('material name',(#16373),#38609);
#16358=REPRESENTATION('density',(#16303),#38609);
#16359=REPRESENTATION('material name',(#16374),#38610);
#16360=REPRESENTATION('density',(#16304),#38610);
#16361=DESCRIPTIVE_REPRESENTATION_ITEM('Aluminum 6061','Aluminum 6061');
#16362=DESCRIPTIVE_REPRESENTATION_ITEM('Aluminum 6061','Aluminum 6061');
#16363=DESCRIPTIVE_REPRESENTATION_ITEM('Aluminum 6061','Aluminum 6061');
#16364=DESCRIPTIVE_REPRESENTATION_ITEM('Aluminum 6061','Aluminum 6061');
#16365=DESCRIPTIVE_REPRESENTATION_ITEM('Silicon Nitride',
'Silicon Nitride');
#16366=DESCRIPTIVE_REPRESENTATION_ITEM('Aluminum 6061','Aluminum 6061');
#16367=DESCRIPTIVE_REPRESENTATION_ITEM('Steel','Steel');
#16368=DESCRIPTIVE_REPRESENTATION_ITEM('Steel','Steel');
#16369=DESCRIPTIVE_REPRESENTATION_ITEM('Aluminum 6061','Aluminum 6061');
#16370=DESCRIPTIVE_REPRESENTATION_ITEM('Brass','Brass');
#16371=DESCRIPTIVE_REPRESENTATION_ITEM('Steel','Steel');
#16372=DESCRIPTIVE_REPRESENTATION_ITEM('Steel','Steel');
#16373=DESCRIPTIVE_REPRESENTATION_ITEM('Steel','Steel');
#16374=DESCRIPTIVE_REPRESENTATION_ITEM('Brass','Brass');
#16375=PROPERTY_DEFINITION('material property','material name',#38684);
#16376=PROPERTY_DEFINITION('material property','density of part',#38684);
#16377=PROPERTY_DEFINITION('material property','material name',#38685);
#16378=PROPERTY_DEFINITION('material property','density of part',#38685);
#16379=PROPERTY_DEFINITION('material property','material name',#38686);
#16380=PROPERTY_DEFINITION('material property','density of part',#38686);
#16381=PROPERTY_DEFINITION('material property','material name',#38687);
#16382=PROPERTY_DEFINITION('material property','density of part',#38687);
#16383=PROPERTY_DEFINITION('material property','material name',#38688);
#16384=PROPERTY_DEFINITION('material property','density of part',#38688);
#16385=PROPERTY_DEFINITION('material property','material name',#38689);
#16386=PROPERTY_DEFINITION('material property','density of part',#38689);
#16387=PROPERTY_DEFINITION('material property','material name',#38690);
#16388=PROPERTY_DEFINITION('material property','density of part',#38690);
#16389=PROPERTY_DEFINITION('material property','material name',#38691);
#16390=PROPERTY_DEFINITION('material property','density of part',#38691);
#16391=PROPERTY_DEFINITION('material property','material name',#38692);
#16392=PROPERTY_DEFINITION('material property','density of part',#38692);
#16393=PROPERTY_DEFINITION('material property','material name',#38693);
#16394=PROPERTY_DEFINITION('material property','density of part',#38693);
#16395=PROPERTY_DEFINITION('material property','material name',#38694);
#16396=PROPERTY_DEFINITION('material property','density of part',#38694);
#16397=PROPERTY_DEFINITION('material property','material name',#38695);
#16398=PROPERTY_DEFINITION('material property','density of part',#38695);
#16399=PROPERTY_DEFINITION('material property','material name',#38696);
#16400=PROPERTY_DEFINITION('material property','density of part',#38696);
#16401=PROPERTY_DEFINITION('material property','material name',#38697);
#16402=PROPERTY_DEFINITION('material property','density of part',#38697);
#16403=AXIS2_PLACEMENT_3D('',#21833,#17805,#17806);
#16404=AXIS2_PLACEMENT_3D('',#21834,#17807,#17808);
#16405=AXIS2_PLACEMENT_3D('',#21835,#17809,#17810);
#16406=AXIS2_PLACEMENT_3D('',#21848,#17817,#17818);
#16407=AXIS2_PLACEMENT_3D('',#21856,#17823,#17824);
#16408=AXIS2_PLACEMENT_3D('',#21864,#17829,#17830);
#16409=AXIS2_PLACEMENT_3D('',#21868,#17833,#17834);
#16410=AXIS2_PLACEMENT_3D('',#21876,#17839,#17840);
#16411=AXIS2_PLACEMENT_3D('',#21882,#17844,#17845);
#16412=AXIS2_PLACEMENT_3D('',#21895,#17852,#17853);
#16413=AXIS2_PLACEMENT_3D('',#21901,#17857,#17858);
#16414=AXIS2_PLACEMENT_3D('',#21907,#17862,#17863);
#16415=AXIS2_PLACEMENT_3D('',#21913,#17867,#17868);
#16416=AXIS2_PLACEMENT_3D('',#21926,#17875,#17876);
#16417=AXIS2_PLACEMENT_3D('',#21934,#17881,#17882);
#16418=AXIS2_PLACEMENT_3D('',#21938,#17885,#17886);
#16419=AXIS2_PLACEMENT_3D('',#21944,#17890,#17891);
#16420=AXIS2_PLACEMENT_3D('',#21957,#17898,#17899);
#16421=AXIS2_PLACEMENT_3D('',#21967,#17905,#17906);
#16422=AXIS2_PLACEMENT_3D('',#21971,#17909,#17910);
#16423=AXIS2_PLACEMENT_3D('',#21979,#17915,#17916);
#16424=AXIS2_PLACEMENT_3D('',#21985,#17920,#17921);
#16425=AXIS2_PLACEMENT_3D('',#21987,#17922,#17923);
#16426=AXIS2_PLACEMENT_3D('',#21990,#17925,#17926);
#16427=AXIS2_PLACEMENT_3D('',#21991,#17927,#17928);
#16428=AXIS2_PLACEMENT_3D('',#21994,#17930,#17931);
#16429=AXIS2_PLACEMENT_3D('',#21995,#17932,#17933);
#16430=AXIS2_PLACEMENT_3D('',#21997,#17934,#17935);
#16431=AXIS2_PLACEMENT_3D('',#21998,#17936,#17937);
#16432=AXIS2_PLACEMENT_3D('',#22001,#17939,#17940);
#16433=AXIS2_PLACEMENT_3D('',#22002,#17941,#17942);
#16434=AXIS2_PLACEMENT_3D('',#22005,#17944,#17945);
#16435=AXIS2_PLACEMENT_3D('',#22146,#17947,#17948);
#16436=AXIS2_PLACEMENT_3D('',#22172,#17950,#17951);
#16437=AXIS2_PLACEMENT_3D('',#22185,#17958,#17959);
#16438=AXIS2_PLACEMENT_3D('',#22191,#17963,#17964);
#16439=AXIS2_PLACEMENT_3D('',#22199,#17969,#17970);
#16440=AXIS2_PLACEMENT_3D('',#22205,#17974,#17975);
#16441=AXIS2_PLACEMENT_3D('',#22218,#17982,#17983);
#16442=AXIS2_PLACEMENT_3D('',#22226,#17988,#17989);
#16443=AXIS2_PLACEMENT_3D('',#22230,#17992,#17993);
#16444=AXIS2_PLACEMENT_3D('',#22236,#17997,#17998);
#16445=AXIS2_PLACEMENT_3D('',#22240,#18000,#18001);
#16446=AXIS2_PLACEMENT_3D('',#22241,#18002,#18003);
#16447=AXIS2_PLACEMENT_3D('',#22242,#18004,#18005);
#16448=AXIS2_PLACEMENT_3D('',#22248,#18009,#18010);
#16449=AXIS2_PLACEMENT_3D('',#22249,#18011,#18012);
#16450=AXIS2_PLACEMENT_3D('',#22250,#18013,#18014);
#16451=AXIS2_PLACEMENT_3D('',#22251,#18015,#18016);
#16452=AXIS2_PLACEMENT_3D('',#22259,#18021,#18022);
#16453=AXIS2_PLACEMENT_3D('',#22263,#18025,#18026);
#16454=AXIS2_PLACEMENT_3D('',#22266,#18028,#18029);
#16455=AXIS2_PLACEMENT_3D('',#22267,#18030,#18031);
#16456=AXIS2_PLACEMENT_3D('',#22271,#18034,#18035);
#16457=AXIS2_PLACEMENT_3D('',#22274,#18037,#18038);
#16458=AXIS2_PLACEMENT_3D('',#22275,#18039,#18040);
#16459=AXIS2_PLACEMENT_3D('',#22277,#18042,#18043);
#16460=AXIS2_PLACEMENT_3D('',#22285,#18048,#18049);
#16461=AXIS2_PLACEMENT_3D('',#22289,#18051,#18052);
#16462=AXIS2_PLACEMENT_3D('',#22290,#18053,#18054);
#16463=AXIS2_PLACEMENT_3D('',#22291,#18055,#18056);
#16464=AXIS2_PLACEMENT_3D('',#22297,#18060,#18061);
#16465=AXIS2_PLACEMENT_3D('',#22301,#18063,#18064);
#16466=AXIS2_PLACEMENT_3D('',#22302,#18065,#18066);
#16467=AXIS2_PLACEMENT_3D('',#22303,#18067,#18068);
#16468=AXIS2_PLACEMENT_3D('',#22308,#18072,#18073);
#16469=AXIS2_PLACEMENT_3D('',#22310,#18075,#18076);
#16470=AXIS2_PLACEMENT_3D('',#22312,#18078,#18079);
#16471=AXIS2_PLACEMENT_3D('',#22314,#18081,#18082);
#16472=AXIS2_PLACEMENT_3D('',#22316,#18084,#18085);
#16473=AXIS2_PLACEMENT_3D('',#22317,#18086,#18087);
#16474=AXIS2_PLACEMENT_3D('',#22321,#18090,#18091);
#16475=AXIS2_PLACEMENT_3D('',#22324,#18093,#18094);
#16476=AXIS2_PLACEMENT_3D('',#22325,#18095,#18096);
#16477=AXIS2_PLACEMENT_3D('',#22326,#18097,#18098);
#16478=AXIS2_PLACEMENT_3D('',#22330,#18101,#18102);
#16479=AXIS2_PLACEMENT_3D('',#22334,#18105,#18106);
#16480=AXIS2_PLACEMENT_3D('',#22338,#18109,#18110);
#16481=AXIS2_PLACEMENT_3D('',#22341,#18112,#18113);
#16482=AXIS2_PLACEMENT_3D('',#22342,#18114,#18115);
#16483=AXIS2_PLACEMENT_3D('',#22343,#18116,#18117);
#16484=AXIS2_PLACEMENT_3D('',#22347,#18120,#18121);
#16485=AXIS2_PLACEMENT_3D('',#22351,#18124,#18125);
#16486=AXIS2_PLACEMENT_3D('',#22355,#18127,#18128);
#16487=AXIS2_PLACEMENT_3D('',#22356,#18129,#18130);
#16488=AXIS2_PLACEMENT_3D('',#22357,#18131,#18132);
#16489=AXIS2_PLACEMENT_3D('',#22363,#18136,#18137);
#16490=AXIS2_PLACEMENT_3D('',#22366,#18139,#18140);
#16491=AXIS2_PLACEMENT_3D('',#22367,#18141,#18142);
#16492=AXIS2_PLACEMENT_3D('',#22368,#18143,#18144);
#16493=AXIS2_PLACEMENT_3D('',#22372,#18147,#18148);
#16494=AXIS2_PLACEMENT_3D('',#22378,#18152,#18153);
#16495=AXIS2_PLACEMENT_3D('',#22382,#18155,#18156);
#16496=AXIS2_PLACEMENT_3D('',#22383,#18157,#18158);
#16497=AXIS2_PLACEMENT_3D('',#22384,#18159,#18160);
#16498=AXIS2_PLACEMENT_3D('',#22389,#18164,#18165);
#16499=AXIS2_PLACEMENT_3D('',#22393,#18168,#18169);
#16500=AXIS2_PLACEMENT_3D('',#22399,#18173,#18174);
#16501=AXIS2_PLACEMENT_3D('',#22402,#18176,#18177);
#16502=AXIS2_PLACEMENT_3D('',#22403,#18178,#18179);
#16503=AXIS2_PLACEMENT_3D('',#22404,#18180,#18181);
#16504=AXIS2_PLACEMENT_3D('',#22406,#18183,#18184);
#16505=AXIS2_PLACEMENT_3D('',#22408,#18185,#18186);
#16506=AXIS2_PLACEMENT_3D('',#22501,#18188,#18189);
#16507=AXIS2_PLACEMENT_3D('',#22503,#18190,#18191);
#16508=AXIS2_PLACEMENT_3D('',#22507,#18193,#18194);
#16509=AXIS2_PLACEMENT_3D('',#22508,#18195,#18196);
#16510=AXIS2_PLACEMENT_3D('',#22509,#18197,#18198);
#16511=AXIS2_PLACEMENT_3D('',#22511,#18199,#18200);
#16512=AXIS2_PLACEMENT_3D('',#22513,#18202,#18203);
#16513=AXIS2_PLACEMENT_3D('',#22515,#18205,#18206);
#16514=AXIS2_PLACEMENT_3D('',#22516,#18207,#18208);
#16515=AXIS2_PLACEMENT_3D('',#22517,#18209,#18210);
#16516=AXIS2_PLACEMENT_3D('',#22518,#18211,#18212);
#16517=AXIS2_PLACEMENT_3D('',#22524,#18216,#18217);
#16518=AXIS2_PLACEMENT_3D('',#22530,#18221,#18222);
#16519=AXIS2_PLACEMENT_3D('',#22534,#18224,#18225);
#16520=AXIS2_PLACEMENT_3D('',#22535,#18226,#18227);
#16521=AXIS2_PLACEMENT_3D('',#22536,#18228,#18229);
#16522=AXIS2_PLACEMENT_3D('',#22542,#18233,#18234);
#16523=AXIS2_PLACEMENT_3D('',#22545,#18236,#18237);
#16524=AXIS2_PLACEMENT_3D('',#22546,#18238,#18239);
#16525=AXIS2_PLACEMENT_3D('',#22547,#18240,#18241);
#16526=AXIS2_PLACEMENT_3D('',#22551,#18244,#18245);
#16527=AXIS2_PLACEMENT_3D('',#22557,#18249,#18250);
#16528=AXIS2_PLACEMENT_3D('',#22561,#18252,#18253);
#16529=AXIS2_PLACEMENT_3D('',#22562,#18254,#18255);
#16530=AXIS2_PLACEMENT_3D('',#22563,#18256,#18257);
#16531=AXIS2_PLACEMENT_3D('',#22566,#18260,#18261);
#16532=AXIS2_PLACEMENT_3D('',#22572,#18265,#18266);
#16533=AXIS2_PLACEMENT_3D('',#22576,#18268,#18269);
#16534=AXIS2_PLACEMENT_3D('',#22577,#18270,#18271);
#16535=AXIS2_PLACEMENT_3D('',#22578,#18272,#18273);
#16536=AXIS2_PLACEMENT_3D('',#22581,#18276,#18277);
#16537=AXIS2_PLACEMENT_3D('',#22587,#18281,#18282);
#16538=AXIS2_PLACEMENT_3D('',#22590,#18284,#18285);
#16539=AXIS2_PLACEMENT_3D('',#22591,#18286,#18287);
#16540=AXIS2_PLACEMENT_3D('',#22592,#18288,#18289);
#16541=AXIS2_PLACEMENT_3D('',#22594,#18291,#18292);
#16542=AXIS2_PLACEMENT_3D('',#22598,#18295,#18296);
#16543=AXIS2_PLACEMENT_3D('',#22602,#18298,#18299);
#16544=AXIS2_PLACEMENT_3D('',#22603,#18300,#18301);
#16545=AXIS2_PLACEMENT_3D('',#22604,#18302,#18303);
#16546=AXIS2_PLACEMENT_3D('',#22607,#18306,#18307);
#16547=AXIS2_PLACEMENT_3D('',#22610,#18309,#18310);
#16548=AXIS2_PLACEMENT_3D('',#22611,#18311,#18312);
#16549=AXIS2_PLACEMENT_3D('',#22615,#18315,#18316);
#16550=AXIS2_PLACEMENT_3D('',#22616,#18317,#18318);
#16551=AXIS2_PLACEMENT_3D('',#22617,#18319,#18320);
#16552=AXIS2_PLACEMENT_3D('',#22620,#18322,#18323);
#16553=AXIS2_PLACEMENT_3D('',#22621,#18324,#18325);
#16554=AXIS2_PLACEMENT_3D('',#22623,#18327,#18328);
#16555=AXIS2_PLACEMENT_3D('',#22627,#18331,#18332);
#16556=AXIS2_PLACEMENT_3D('',#22630,#18334,#18335);
#16557=AXIS2_PLACEMENT_3D('',#22631,#18336,#18337);
#16558=AXIS2_PLACEMENT_3D('',#22633,#18339,#18340);
#16559=AXIS2_PLACEMENT_3D('',#22634,#18341,#18342);
#16560=AXIS2_PLACEMENT_3D('',#22636,#18343,#18344);
#16561=AXIS2_PLACEMENT_3D('',#22638,#18346,#18347);
#16562=AXIS2_PLACEMENT_3D('',#22642,#18350,#18351);
#16563=AXIS2_PLACEMENT_3D('',#22643,#18352,#18353);
#16564=AXIS2_PLACEMENT_3D('',#22644,#18354,#18355);
#16565=AXIS2_PLACEMENT_3D('',#22646,#18357,#18358);
#16566=AXIS2_PLACEMENT_3D('',#22648,#18360,#18361);
#16567=AXIS2_PLACEMENT_3D('',#22649,#18362,#18363);
#16568=AXIS2_PLACEMENT_3D('',#22650,#18364,#18365);
#16569=AXIS2_PLACEMENT_3D('',#22651,#18366,#18367);
#16570=AXIS2_PLACEMENT_3D('',#22653,#18369,#18370);
#16571=AXIS2_PLACEMENT_3D('',#22654,#18371,#18372);
#16572=AXIS2_PLACEMENT_3D('',#22655,#18373,#18374);
#16573=AXIS2_PLACEMENT_3D('',#22656,#18375,#18376);
#16574=AXIS2_PLACEMENT_3D('',#22658,#18378,#18379);
#16575=AXIS2_PLACEMENT_3D('',#22660,#18381,#18382);
#16576=AXIS2_PLACEMENT_3D('',#22661,#18383,#18384);
#16577=AXIS2_PLACEMENT_3D('',#22663,#18386,#18387);
#16578=AXIS2_PLACEMENT_3D('',#22664,#18388,#18389);
#16579=AXIS2_PLACEMENT_3D('',#22666,#18391,#18392);
#16580=AXIS2_PLACEMENT_3D('',#22668,#18394,#18395);
#16581=AXIS2_PLACEMENT_3D('',#22669,#18396,#18397);
#16582=AXIS2_PLACEMENT_3D('',#22670,#18398,#18399);
#16583=AXIS2_PLACEMENT_3D('',#22672,#18400,#18401);
#16584=AXIS2_PLACEMENT_3D('',#22674,#18402,#18403);
#16585=AXIS2_PLACEMENT_3D('',#22675,#18404,#18405);
#16586=AXIS2_PLACEMENT_3D('',#22677,#18406,#18407);
#16587=AXIS2_PLACEMENT_3D('',#22679,#18409,#18410);
#16588=AXIS2_PLACEMENT_3D('',#22693,#18411,#18412);
#16589=AXIS2_PLACEMENT_3D('',#22718,#18414,#18415);
#16590=AXIS2_PLACEMENT_3D('',#22729,#18416,#18417);
#16591=AXIS2_PLACEMENT_3D('',#22731,#18418,#18419);
#16592=AXIS2_PLACEMENT_3D('',#22734,#18421,#18422);
#16593=AXIS2_PLACEMENT_3D('',#22735,#18423,#18424);
#16594=AXIS2_PLACEMENT_3D('',#22737,#18425,#18426);
#16595=AXIS2_PLACEMENT_3D('',#22738,#18427,#18428);
#16596=AXIS2_PLACEMENT_3D('',#22778,#18430,#18431);
#16597=AXIS2_PLACEMENT_3D('',#22780,#18433,#18434);
#16598=AXIS2_PLACEMENT_3D('',#22782,#18436,#18437);
#16599=AXIS2_PLACEMENT_3D('',#22825,#18439,#18440);
#16600=AXIS2_PLACEMENT_3D('',#22829,#18442,#18443);
#16601=AXIS2_PLACEMENT_3D('',#22830,#18444,#18445);
#16602=AXIS2_PLACEMENT_3D('',#22845,#18447,#18448);
#16603=AXIS2_PLACEMENT_3D('',#22874,#18449,#18450);
#16604=AXIS2_PLACEMENT_3D('',#22876,#18452,#18453);
#16605=AXIS2_PLACEMENT_3D('',#22878,#18454,#18455);
#16606=AXIS2_PLACEMENT_3D('',#22879,#18456,#18457);
#16607=AXIS2_PLACEMENT_3D('',#22881,#18458,#18459);
#16608=AXIS2_PLACEMENT_3D('',#22883,#18461,#18462);
#16609=AXIS2_PLACEMENT_3D('',#22885,#18463,#18464);
#16610=AXIS2_PLACEMENT_3D('',#22887,#18466,#18467);
#16611=AXIS2_PLACEMENT_3D('',#22889,#18468,#18469);
#16612=AXIS2_PLACEMENT_3D('',#22890,#18470,#18471);
#16613=AXIS2_PLACEMENT_3D('',#22892,#18472,#18473);
#16614=AXIS2_PLACEMENT_3D('',#22894,#18475,#18476);
#16615=AXIS2_PLACEMENT_3D('',#22896,#18477,#18478);
#16616=AXIS2_PLACEMENT_3D('',#22899,#18481,#18482);
#16617=AXIS2_PLACEMENT_3D('',#22901,#18483,#18484);
#16618=AXIS2_PLACEMENT_3D('',#22903,#18486,#18487);
#16619=AXIS2_PLACEMENT_3D('',#22905,#18488,#18489);
#16620=AXIS2_PLACEMENT_3D('',#22906,#18490,#18491);
#16621=AXIS2_PLACEMENT_3D('',#22909,#18493,#18494);
#16622=AXIS2_PLACEMENT_3D('',#22910,#18495,#18496);
#16623=AXIS2_PLACEMENT_3D('',#22914,#18499,#18500);
#16624=AXIS2_PLACEMENT_3D('',#22915,#18501,#18502);
#16625=AXIS2_PLACEMENT_3D('',#22916,#18503,#18504);
#16626=AXIS2_PLACEMENT_3D('',#22917,#18505,#18506);
#16627=AXIS2_PLACEMENT_3D('',#22919,#18507,#18508);
#16628=AXIS2_PLACEMENT_3D('',#22923,#18510,#18511);
#16629=AXIS2_PLACEMENT_3D('',#22924,#18512,#18513);
#16630=AXIS2_PLACEMENT_3D('',#22925,#18514,#18515);
#16631=AXIS2_PLACEMENT_3D('',#22929,#18517,#18518);
#16632=AXIS2_PLACEMENT_3D('',#22930,#18519,#18520);
#16633=AXIS2_PLACEMENT_3D('',#22931,#18521,#18522);
#16634=AXIS2_PLACEMENT_3D('',#22932,#18523,#18524);
#16635=AXIS2_PLACEMENT_3D('',#22936,#18526,#18527);
#16636=AXIS2_PLACEMENT_3D('',#22937,#18528,#18529);
#16637=AXIS2_PLACEMENT_3D('',#22938,#18530,#18531);
#16638=AXIS2_PLACEMENT_3D('',#22942,#18533,#18534);
#16639=AXIS2_PLACEMENT_3D('',#22943,#18535,#18536);
#16640=AXIS2_PLACEMENT_3D('',#22944,#18537,#18538);
#16641=AXIS2_PLACEMENT_3D('',#22948,#18540,#18541);
#16642=AXIS2_PLACEMENT_3D('',#22949,#18542,#18543);
#16643=AXIS2_PLACEMENT_3D('',#22950,#18544,#18545);
#16644=AXIS2_PLACEMENT_3D('',#22954,#18547,#18548);
#16645=AXIS2_PLACEMENT_3D('',#22955,#18549,#18550);
#16646=AXIS2_PLACEMENT_3D('',#22956,#18551,#18552);
#16647=AXIS2_PLACEMENT_3D('',#22959,#18554,#18555);
#16648=AXIS2_PLACEMENT_3D('',#22960,#18556,#18557);
#16649=AXIS2_PLACEMENT_3D('',#22961,#18558,#18559);
#16650=AXIS2_PLACEMENT_3D('',#22962,#18560,#18561);
#16651=AXIS2_PLACEMENT_3D('',#22975,#18568,#18569);
#16652=AXIS2_PLACEMENT_3D('',#22985,#18575,#18576);
#16653=AXIS2_PLACEMENT_3D('',#22999,#18584,#18585);
#16654=AXIS2_PLACEMENT_3D('',#23003,#18588,#18589);
#16655=AXIS2_PLACEMENT_3D('',#23013,#18595,#18596);
#16656=AXIS2_PLACEMENT_3D('',#23015,#18598,#18599);
#16657=AXIS2_PLACEMENT_3D('',#23027,#18606,#18607);
#16658=AXIS2_PLACEMENT_3D('',#23033,#18611,#18612);
#16659=AXIS2_PLACEMENT_3D('',#23045,#18619,#18620);
#16660=AXIS2_PLACEMENT_3D('',#23055,#18626,#18627);
#16661=AXIS2_PLACEMENT_3D('',#23065,#18633,#18634);
#16662=AXIS2_PLACEMENT_3D('',#23069,#18637,#18638);
#16663=AXIS2_PLACEMENT_3D('',#23075,#18642,#18643);
#16664=AXIS2_PLACEMENT_3D('',#23079,#18646,#18647);
#16665=AXIS2_PLACEMENT_3D('',#23091,#18654,#18655);
#16666=AXIS2_PLACEMENT_3D('',#23101,#18661,#18662);
#16667=AXIS2_PLACEMENT_3D('',#23111,#18668,#18669);
#16668=AXIS2_PLACEMENT_3D('',#23115,#18672,#18673);
#16669=AXIS2_PLACEMENT_3D('',#23121,#18677,#18678);
#16670=AXIS2_PLACEMENT_3D('',#23127,#18682,#18683);
#16671=AXIS2_PLACEMENT_3D('',#23136,#18689,#18690);
#16672=AXIS2_PLACEMENT_3D('',#23150,#18698,#18699);
#16673=AXIS2_PLACEMENT_3D('',#23154,#18702,#18703);
#16674=AXIS2_PLACEMENT_3D('',#23164,#18709,#18710);
#16675=AXIS2_PLACEMENT_3D('',#23171,#18715,#18716);
#16676=AXIS2_PLACEMENT_3D('',#23175,#18719,#18720);
#16677=AXIS2_PLACEMENT_3D('',#23177,#18722,#18723);
#16678=AXIS2_PLACEMENT_3D('',#23182,#18727,#18728);
#16679=AXIS2_PLACEMENT_3D('',#23185,#18731,#18732);
#16680=AXIS2_PLACEMENT_3D('',#23186,#18733,#18734);
#16681=AXIS2_PLACEMENT_3D('',#23193,#18739,#18740);
#16682=AXIS2_PLACEMENT_3D('',#23197,#18743,#18744);
#16683=AXIS2_PLACEMENT_3D('',#23198,#18745,#18746);
#16684=AXIS2_PLACEMENT_3D('',#23202,#18749,#18750);
#16685=AXIS2_PLACEMENT_3D('',#23205,#18752,#18753);
#16686=AXIS2_PLACEMENT_3D('',#23207,#18754,#18755);
#16687=AXIS2_PLACEMENT_3D('',#23209,#18756,#18757);
#16688=AXIS2_PLACEMENT_3D('',#23211,#18758,#18759);
#16689=AXIS2_PLACEMENT_3D('',#23213,#18760,#18761);
#16690=AXIS2_PLACEMENT_3D('',#23215,#18762,#18763);
#16691=AXIS2_PLACEMENT_3D('',#23216,#18764,#18765);
#16692=AXIS2_PLACEMENT_3D('',#23217,#18766,#18767);
#16693=AXIS2_PLACEMENT_3D('',#23219,#18769,#18770);
#16694=AXIS2_PLACEMENT_3D('',#23223,#18773,#18774);
#16695=AXIS2_PLACEMENT_3D('',#23227,#18777,#18778);
#16696=AXIS2_PLACEMENT_3D('',#23232,#18782,#18783);
#16697=AXIS2_PLACEMENT_3D('',#23235,#18784,#18785);
#16698=AXIS2_PLACEMENT_3D('',#23236,#18786,#18787);
#16699=AXIS2_PLACEMENT_3D('',#23240,#18789,#18790);
#16700=AXIS2_PLACEMENT_3D('',#23241,#18791,#18792);
#16701=AXIS2_PLACEMENT_3D('',#23242,#18793,#18794);
#16702=AXIS2_PLACEMENT_3D('',#23245,#18795,#18796);
#16703=AXIS2_PLACEMENT_3D('',#23246,#18797,#18798);
#16704=AXIS2_PLACEMENT_3D('',#23248,#18800,#18801);
#16705=AXIS2_PLACEMENT_3D('',#23251,#18803,#18804);
#16706=AXIS2_PLACEMENT_3D('',#23252,#18805,#18806);
#16707=AXIS2_PLACEMENT_3D('',#23254,#18807,#18808);
#16708=AXIS2_PLACEMENT_3D('',#23256,#18810,#18811);
#16709=AXIS2_PLACEMENT_3D('',#23258,#18812,#18813);
#16710=AXIS2_PLACEMENT_3D('',#23259,#18814,#18815);
#16711=AXIS2_PLACEMENT_3D('',#23261,#18816,#18817);
#16712=AXIS2_PLACEMENT_3D('',#23265,#18819,#18820);
#16713=AXIS2_PLACEMENT_3D('',#23266,#18821,#18822);
#16714=AXIS2_PLACEMENT_3D('',#23267,#18823,#18824);
#16715=AXIS2_PLACEMENT_3D('',#23269,#18825,#18826);
#16716=AXIS2_PLACEMENT_3D('',#23270,#18827,#18828);
#16717=AXIS2_PLACEMENT_3D('',#23272,#18830,#18831);
#16718=AXIS2_PLACEMENT_3D('',#23275,#18833,#18834);
#16719=AXIS2_PLACEMENT_3D('',#23276,#18835,#18836);
#16720=AXIS2_PLACEMENT_3D('',#23278,#18838,#18839);
#16721=AXIS2_PLACEMENT_3D('',#23281,#18841,#18842);
#16722=AXIS2_PLACEMENT_3D('',#23282,#18843,#18844);
#16723=AXIS2_PLACEMENT_3D('',#23285,#18845,#18846);
#16724=AXIS2_PLACEMENT_3D('',#23286,#18847,#18848);
#16725=AXIS2_PLACEMENT_3D('',#23288,#18850,#18851);
#16726=AXIS2_PLACEMENT_3D('',#23290,#18852,#18853);
#16727=AXIS2_PLACEMENT_3D('',#23292,#18855,#18856);
#16728=AXIS2_PLACEMENT_3D('',#23294,#18857,#18858);
#16729=AXIS2_PLACEMENT_3D('',#23295,#18859,#18860);
#16730=AXIS2_PLACEMENT_3D('',#23298,#18862,#18863);
#16731=AXIS2_PLACEMENT_3D('',#23299,#18864,#18865);
#16732=AXIS2_PLACEMENT_3D('',#23302,#18866,#18867);
#16733=AXIS2_PLACEMENT_3D('',#23303,#18868,#18869);
#16734=AXIS2_PLACEMENT_3D('',#23305,#18871,#18872);
#16735=AXIS2_PLACEMENT_3D('',#23307,#18873,#18874);
#16736=AXIS2_PLACEMENT_3D('',#23309,#18876,#18877);
#16737=AXIS2_PLACEMENT_3D('',#23311,#18878,#18879);
#16738=AXIS2_PLACEMENT_3D('',#23312,#18880,#18881);
#16739=AXIS2_PLACEMENT_3D('',#23315,#18883,#18884);
#16740=AXIS2_PLACEMENT_3D('',#23316,#18885,#18886);
#16741=AXIS2_PLACEMENT_3D('',#23318,#18887,#18888);
#16742=AXIS2_PLACEMENT_3D('',#23320,#18890,#18891);
#16743=AXIS2_PLACEMENT_3D('',#23323,#18893,#18894);
#16744=AXIS2_PLACEMENT_3D('',#23324,#18895,#18896);
#16745=AXIS2_PLACEMENT_3D('',#23326,#18897,#18898);
#16746=AXIS2_PLACEMENT_3D('',#23328,#18900,#18901);
#16747=AXIS2_PLACEMENT_3D('',#23331,#18903,#18904);
#16748=AXIS2_PLACEMENT_3D('',#23332,#18905,#18906);
#16749=AXIS2_PLACEMENT_3D('',#23334,#18907,#18908);
#16750=AXIS2_PLACEMENT_3D('',#23336,#18910,#18911);
#16751=AXIS2_PLACEMENT_3D('',#23338,#18912,#18913);
#16752=AXIS2_PLACEMENT_3D('',#23341,#18915,#18916);
#16753=AXIS2_PLACEMENT_3D('',#23342,#18917,#18918);
#16754=AXIS2_PLACEMENT_3D('',#23352,#18923,#18924);
#16755=AXIS2_PLACEMENT_3D('',#23354,#18925,#18926);
#16756=AXIS2_PLACEMENT_3D('',#23356,#18927,#18928);
#16757=AXIS2_PLACEMENT_3D('',#23358,#18929,#18930);
#16758=AXIS2_PLACEMENT_3D('',#23360,#18931,#18932);
#16759=AXIS2_PLACEMENT_3D('',#23361,#18933,#18934);
#16760=AXIS2_PLACEMENT_3D('',#23363,#18936,#18937);
#16761=AXIS2_PLACEMENT_3D('',#23366,#18939,#18940);
#16762=AXIS2_PLACEMENT_3D('',#23367,#18941,#18942);
#16763=AXIS2_PLACEMENT_3D('',#23369,#18944,#18945);
#16764=AXIS2_PLACEMENT_3D('',#23371,#18947,#18948);
#16765=AXIS2_PLACEMENT_3D('',#23374,#18951,#18952);
#16766=AXIS2_PLACEMENT_3D('',#23376,#18954,#18955);
#16767=AXIS2_PLACEMENT_3D('',#23378,#18957,#18958);
#16768=AXIS2_PLACEMENT_3D('',#23379,#18959,#18960);
#16769=AXIS2_PLACEMENT_3D('',#23381,#18962,#18963);
#16770=AXIS2_PLACEMENT_3D('',#23383,#18965,#18966);
#16771=AXIS2_PLACEMENT_3D('',#23385,#18968,#18969);
#16772=AXIS2_PLACEMENT_3D('',#23386,#18970,#18971);
#16773=AXIS2_PLACEMENT_3D('',#23387,#18972,#18973);
#16774=AXIS2_PLACEMENT_3D('',#23388,#18974,#18975);
#16775=AXIS2_PLACEMENT_3D('',#23389,#18976,#18977);
#16776=AXIS2_PLACEMENT_3D('',#23391,#18978,#18979);
#16777=AXIS2_PLACEMENT_3D('',#23392,#18980,#18981);
#16778=AXIS2_PLACEMENT_3D('',#23394,#18982,#18983);
#16779=AXIS2_PLACEMENT_3D('',#23396,#18985,#18986);
#16780=AXIS2_PLACEMENT_3D('',#23398,#18987,#18988);
#16781=AXIS2_PLACEMENT_3D('',#23400,#18990,#18991);
#16782=AXIS2_PLACEMENT_3D('',#23402,#18992,#18993);
#16783=AXIS2_PLACEMENT_3D('',#23404,#18995,#18996);
#16784=AXIS2_PLACEMENT_3D('',#23405,#18997,#18998);
#16785=AXIS2_PLACEMENT_3D('',#23406,#18999,#19000);
#16786=AXIS2_PLACEMENT_3D('',#23499,#19003,#19004);
#16787=AXIS2_PLACEMENT_3D('',#23589,#19006,#19007);
#16788=AXIS2_PLACEMENT_3D('',#23609,#19009,#19010);
#16789=AXIS2_PLACEMENT_3D('',#23621,#19011,#19012);
#16790=AXIS2_PLACEMENT_3D('',#23626,#19014,#19015);
#16791=AXIS2_PLACEMENT_3D('',#23990,#19016,#19017);
#16792=AXIS2_PLACEMENT_3D('',#23995,#19019,#19020);
#16793=AXIS2_PLACEMENT_3D('',#24039,#19021,#19022);
#16794=AXIS2_PLACEMENT_3D('',#24043,#19024,#19025);
#16795=AXIS2_PLACEMENT_3D('',#24081,#19027,#19028);
#16796=AXIS2_PLACEMENT_3D('',#24082,#19029,#19030);
#16797=AXIS2_PLACEMENT_3D('',#24121,#19032,#19033);
#16798=AXIS2_PLACEMENT_3D('',#24448,#19034,#19035);
#16799=AXIS2_PLACEMENT_3D('',#24452,#19038,#19039);
#16800=AXIS2_PLACEMENT_3D('',#24453,#19040,#19041);
#16801=AXIS2_PLACEMENT_3D('',#24455,#19043,#19044);
#16802=AXIS2_PLACEMENT_3D('',#24457,#19045,#19046);
#16803=AXIS2_PLACEMENT_3D('',#24458,#19047,#19048);
#16804=AXIS2_PLACEMENT_3D('',#24493,#19049,#19050);
#16805=AXIS2_PLACEMENT_3D('',#24507,#19054,#19055);
#16806=AXIS2_PLACEMENT_3D('',#24521,#19059,#19060);
#16807=AXIS2_PLACEMENT_3D('',#24522,#19061,#19062);
#16808=AXIS2_PLACEMENT_3D('',#24523,#19063,#19064);
#16809=AXIS2_PLACEMENT_3D('',#24525,#19066,#19067);
#16810=AXIS2_PLACEMENT_3D('',#24526,#19068,#19069);
#16811=AXIS2_PLACEMENT_3D('',#24530,#19071,#19072);
#16812=AXIS2_PLACEMENT_3D('',#24531,#19073,#19074);
#16813=AXIS2_PLACEMENT_3D('',#24532,#19075,#19076);
#16814=AXIS2_PLACEMENT_3D('',#24544,#19079,#19080);
#16815=AXIS2_PLACEMENT_3D('',#24546,#19081,#19082);
#16816=AXIS2_PLACEMENT_3D('',#24548,#19084,#19085);
#16817=AXIS2_PLACEMENT_3D('',#24560,#19088,#19089);
#16818=AXIS2_PLACEMENT_3D('',#24562,#19090,#19091);
#16819=AXIS2_PLACEMENT_3D('',#24564,#19093,#19094);
#16820=AXIS2_PLACEMENT_3D('',#24565,#19095,#19096);
#16821=AXIS2_PLACEMENT_3D('',#24566,#19097,#19098);
#16822=AXIS2_PLACEMENT_3D('',#24567,#19099,#19100);
#16823=AXIS2_PLACEMENT_3D('',#24568,#19101,#19102);
#16824=AXIS2_PLACEMENT_3D('',#24569,#19103,#19104);
#16825=AXIS2_PLACEMENT_3D('',#24570,#19105,#19106);
#16826=AXIS2_PLACEMENT_3D('',#24571,#19107,#19108);
#16827=AXIS2_PLACEMENT_3D('',#24572,#19109,#19110);
#16828=AXIS2_PLACEMENT_3D('',#24573,#19111,#19112);
#16829=AXIS2_PLACEMENT_3D('',#24574,#19113,#19114);
#16830=AXIS2_PLACEMENT_3D('',#24575,#19115,#19116);
#16831=AXIS2_PLACEMENT_3D('',#24576,#19117,#19118);
#16832=AXIS2_PLACEMENT_3D('',#24578,#19119,#19120);
#16833=AXIS2_PLACEMENT_3D('',#24580,#19122,#19123);
#16834=AXIS2_PLACEMENT_3D('',#24581,#19124,#19125);
#16835=AXIS2_PLACEMENT_3D('',#24582,#19126,#19127);
#16836=AXIS2_PLACEMENT_3D('',#24598,#19129,#19130);
#16837=AXIS2_PLACEMENT_3D('',#24606,#19131,#19132);
#16838=AXIS2_PLACEMENT_3D('',#24654,#19134,#19135);
#16839=AXIS2_PLACEMENT_3D('',#24702,#19137,#19138);
#16840=AXIS2_PLACEMENT_3D('',#24756,#19140,#19141);
#16841=AXIS2_PLACEMENT_3D('',#24804,#19143,#19144);
#16842=AXIS2_PLACEMENT_3D('',#24852,#19146,#19147);
#16843=AXIS2_PLACEMENT_3D('',#24865,#19149,#19150);
#16844=AXIS2_PLACEMENT_3D('',#24871,#19151,#19152);
#16845=AXIS2_PLACEMENT_3D('',#24896,#19154,#19155);
#16846=AXIS2_PLACEMENT_3D('',#24920,#19157,#19158);
#16847=AXIS2_PLACEMENT_3D('',#24945,#19160,#19161);
#16848=AXIS2_PLACEMENT_3D('',#24970,#19163,#19164);
#16849=AXIS2_PLACEMENT_3D('',#24994,#19166,#19167);
#16850=AXIS2_PLACEMENT_3D('',#25049,#19168,#19169);
#16851=AXIS2_PLACEMENT_3D('',#25051,#19170,#19171);
#16852=AXIS2_PLACEMENT_3D('',#25367,#19172,#19173);
#16853=AXIS2_PLACEMENT_3D('',#25369,#19174,#19175);
#16854=AXIS2_PLACEMENT_3D('',#25370,#19176,#19177);
#16855=AXIS2_PLACEMENT_3D('',#25427,#19178,#19179);
#16856=AXIS2_PLACEMENT_3D('',#25428,#19180,#19181);
#16857=AXIS2_PLACEMENT_3D('',#25632,#19182,#19183);
#16858=AXIS2_PLACEMENT_3D('',#25636,#19185,#19186);
#16859=AXIS2_PLACEMENT_3D('',#25637,#19187,#19188);
#16860=AXIS2_PLACEMENT_3D('',#25640,#19190,#19191);
#16861=AXIS2_PLACEMENT_3D('',#25641,#19192,#19193);
#16862=AXIS2_PLACEMENT_3D('',#25644,#19195,#19196);
#16863=AXIS2_PLACEMENT_3D('',#25645,#19197,#19198);
#16864=AXIS2_PLACEMENT_3D('',#25648,#19200,#19201);
#16865=AXIS2_PLACEMENT_3D('',#25649,#19202,#19203);
#16866=AXIS2_PLACEMENT_3D('',#25652,#19205,#19206);
#16867=AXIS2_PLACEMENT_3D('',#25653,#19207,#19208);
#16868=AXIS2_PLACEMENT_3D('',#25655,#19210,#19211);
#16869=AXIS2_PLACEMENT_3D('',#25656,#19212,#19213);
#16870=AXIS2_PLACEMENT_3D('',#25661,#19215,#19216);
#16871=AXIS2_PLACEMENT_3D('',#25670,#19217,#19218);
#16872=AXIS2_PLACEMENT_3D('',#25679,#19219,#19220);
#16873=AXIS2_PLACEMENT_3D('',#25688,#19221,#19222);
#16874=AXIS2_PLACEMENT_3D('',#25697,#19223,#19224);
#16875=AXIS2_PLACEMENT_3D('',#25706,#19225,#19226);
#16876=AXIS2_PLACEMENT_3D('',#25714,#19227,#19228);
#16877=AXIS2_PLACEMENT_3D('',#25715,#19229,#19230);
#16878=AXIS2_PLACEMENT_3D('',#25721,#19234,#19235);
#16879=AXIS2_PLACEMENT_3D('',#25725,#19238,#19239);
#16880=AXIS2_PLACEMENT_3D('',#25729,#19242,#19243);
#16881=AXIS2_PLACEMENT_3D('',#25733,#19246,#19247);
#16882=AXIS2_PLACEMENT_3D('',#25737,#19250,#19251);
#16883=AXIS2_PLACEMENT_3D('',#25741,#19254,#19255);
#16884=AXIS2_PLACEMENT_3D('',#25745,#19258,#19259);
#16885=AXIS2_PLACEMENT_3D('',#25749,#19262,#19263);
#16886=AXIS2_PLACEMENT_3D('',#25753,#19266,#19267);
#16887=AXIS2_PLACEMENT_3D('',#25755,#19269,#19270);
#16888=AXIS2_PLACEMENT_3D('',#25757,#19272,#19273);
#16889=AXIS2_PLACEMENT_3D('',#25758,#19274,#19275);
#16890=AXIS2_PLACEMENT_3D('',#25760,#19277,#19278);
#16891=AXIS2_PLACEMENT_3D('',#25764,#19281,#19282);
#16892=AXIS2_PLACEMENT_3D('',#25766,#19284,#19285);
#16893=AXIS2_PLACEMENT_3D('',#25768,#19287,#19288);
#16894=AXIS2_PLACEMENT_3D('',#25772,#19291,#19292);
#16895=AXIS2_PLACEMENT_3D('',#25774,#19294,#19295);
#16896=AXIS2_PLACEMENT_3D('',#25775,#19296,#19297);
#16897=AXIS2_PLACEMENT_3D('',#25776,#19298,#19299);
#16898=AXIS2_PLACEMENT_3D('',#25778,#19301,#19302);
#16899=AXIS2_PLACEMENT_3D('',#25779,#19303,#19304);
#16900=AXIS2_PLACEMENT_3D('',#25780,#19305,#19306);
#16901=AXIS2_PLACEMENT_3D('',#25781,#19307,#19308);
#16902=AXIS2_PLACEMENT_3D('',#25783,#19309,#19310);
#16903=AXIS2_PLACEMENT_3D('',#25784,#19311,#19312);
#16904=AXIS2_PLACEMENT_3D('',#25786,#19314,#19315);
#16905=AXIS2_PLACEMENT_3D('',#25787,#19316,#19317);
#16906=AXIS2_PLACEMENT_3D('',#25788,#19318,#19319);
#16907=AXIS2_PLACEMENT_3D('',#25790,#19320,#19321);
#16908=AXIS2_PLACEMENT_3D('',#25792,#19323,#19324);
#16909=AXIS2_PLACEMENT_3D('',#25793,#19325,#19326);
#16910=AXIS2_PLACEMENT_3D('',#25794,#19327,#19328);
#16911=AXIS2_PLACEMENT_3D('',#25810,#19330,#19331);
#16912=AXIS2_PLACEMENT_3D('',#25818,#19332,#19333);
#16913=AXIS2_PLACEMENT_3D('',#25866,#19335,#19336);
#16914=AXIS2_PLACEMENT_3D('',#25914,#19338,#19339);
#16915=AXIS2_PLACEMENT_3D('',#25968,#19341,#19342);
#16916=AXIS2_PLACEMENT_3D('',#26016,#19344,#19345);
#16917=AXIS2_PLACEMENT_3D('',#26025,#19347,#19348);
#16918=AXIS2_PLACEMENT_3D('',#26026,#19349,#19350);
#16919=AXIS2_PLACEMENT_3D('',#26041,#19352,#19353);
#16920=AXIS2_PLACEMENT_3D('',#26051,#19354,#19355);
#16921=AXIS2_PLACEMENT_3D('',#26076,#19357,#19358);
#16922=AXIS2_PLACEMENT_3D('',#26101,#19360,#19361);
#16923=AXIS2_PLACEMENT_3D('',#26125,#19363,#19364);
#16924=AXIS2_PLACEMENT_3D('',#26180,#19365,#19366);
#16925=AXIS2_PLACEMENT_3D('',#26182,#19367,#19368);
#16926=AXIS2_PLACEMENT_3D('',#26453,#19369,#19370);
#16927=AXIS2_PLACEMENT_3D('',#26455,#19371,#19372);
#16928=AXIS2_PLACEMENT_3D('',#26456,#19373,#19374);
#16929=AXIS2_PLACEMENT_3D('',#26513,#19375,#19376);
#16930=AXIS2_PLACEMENT_3D('',#26514,#19377,#19378);
#16931=AXIS2_PLACEMENT_3D('',#26673,#19379,#19380);
#16932=AXIS2_PLACEMENT_3D('',#26677,#19382,#19383);
#16933=AXIS2_PLACEMENT_3D('',#26678,#19384,#19385);
#16934=AXIS2_PLACEMENT_3D('',#26681,#19387,#19388);
#16935=AXIS2_PLACEMENT_3D('',#26682,#19389,#19390);
#16936=AXIS2_PLACEMENT_3D('',#26685,#19392,#19393);
#16937=AXIS2_PLACEMENT_3D('',#26686,#19394,#19395);
#16938=AXIS2_PLACEMENT_3D('',#26689,#19397,#19398);
#16939=AXIS2_PLACEMENT_3D('',#26690,#19399,#19400);
#16940=AXIS2_PLACEMENT_3D('',#26693,#19402,#19403);
#16941=AXIS2_PLACEMENT_3D('',#26694,#19404,#19405);
#16942=AXIS2_PLACEMENT_3D('',#26696,#19407,#19408);
#16943=AXIS2_PLACEMENT_3D('',#26697,#19409,#19410);
#16944=AXIS2_PLACEMENT_3D('',#26702,#19412,#19413);
#16945=AXIS2_PLACEMENT_3D('',#26711,#19414,#19415);
#16946=AXIS2_PLACEMENT_3D('',#26720,#19416,#19417);
#16947=AXIS2_PLACEMENT_3D('',#26729,#19418,#19419);
#16948=AXIS2_PLACEMENT_3D('',#26738,#19420,#19421);
#16949=AXIS2_PLACEMENT_3D('',#26747,#19422,#19423);
#16950=AXIS2_PLACEMENT_3D('',#26755,#19424,#19425);
#16951=AXIS2_PLACEMENT_3D('',#26756,#19426,#19427);
#16952=AXIS2_PLACEMENT_3D('',#26762,#19431,#19432);
#16953=AXIS2_PLACEMENT_3D('',#26766,#19435,#19436);
#16954=AXIS2_PLACEMENT_3D('',#26770,#19439,#19440);
#16955=AXIS2_PLACEMENT_3D('',#26774,#19443,#19444);
#16956=AXIS2_PLACEMENT_3D('',#26778,#19447,#19448);
#16957=AXIS2_PLACEMENT_3D('',#26782,#19451,#19452);
#16958=AXIS2_PLACEMENT_3D('',#26786,#19455,#19456);
#16959=AXIS2_PLACEMENT_3D('',#26790,#19459,#19460);
#16960=AXIS2_PLACEMENT_3D('',#26794,#19463,#19464);
#16961=AXIS2_PLACEMENT_3D('',#26796,#19466,#19467);
#16962=AXIS2_PLACEMENT_3D('',#26798,#19469,#19470);
#16963=AXIS2_PLACEMENT_3D('',#26799,#19471,#19472);
#16964=AXIS2_PLACEMENT_3D('',#26801,#19474,#19475);
#16965=AXIS2_PLACEMENT_3D('',#26805,#19478,#19479);
#16966=AXIS2_PLACEMENT_3D('',#26807,#19481,#19482);
#16967=AXIS2_PLACEMENT_3D('',#26809,#19484,#19485);
#16968=AXIS2_PLACEMENT_3D('',#26813,#19488,#19489);
#16969=AXIS2_PLACEMENT_3D('',#26815,#19491,#19492);
#16970=AXIS2_PLACEMENT_3D('',#26816,#19493,#19494);
#16971=AXIS2_PLACEMENT_3D('',#26817,#19495,#19496);
#16972=AXIS2_PLACEMENT_3D('',#26819,#19498,#19499);
#16973=AXIS2_PLACEMENT_3D('',#26820,#19500,#19501);
#16974=AXIS2_PLACEMENT_3D('',#26821,#19502,#19503);
#16975=AXIS2_PLACEMENT_3D('',#26822,#19504,#19505);
#16976=AXIS2_PLACEMENT_3D('',#26824,#19506,#19507);
#16977=AXIS2_PLACEMENT_3D('',#26825,#19508,#19509);
#16978=AXIS2_PLACEMENT_3D('',#26827,#19511,#19512);
#16979=AXIS2_PLACEMENT_3D('',#26828,#19513,#19514);
#16980=AXIS2_PLACEMENT_3D('',#26829,#19515,#19516);
#16981=AXIS2_PLACEMENT_3D('',#26831,#19517,#19518);
#16982=AXIS2_PLACEMENT_3D('',#26833,#19520,#19521);
#16983=AXIS2_PLACEMENT_3D('',#26834,#19522,#19523);
#16984=AXIS2_PLACEMENT_3D('',#26835,#19524,#19525);
#16985=AXIS2_PLACEMENT_3D('',#26848,#19532,#19533);
#16986=AXIS2_PLACEMENT_3D('',#26856,#19538,#19539);
#16987=AXIS2_PLACEMENT_3D('',#26862,#19543,#19544);
#16988=AXIS2_PLACEMENT_3D('',#26868,#19548,#19549);
#16989=AXIS2_PLACEMENT_3D('',#26877,#19554,#19555);
#16990=AXIS2_PLACEMENT_3D('',#26883,#19559,#19560);
#16991=AXIS2_PLACEMENT_3D('',#26889,#19564,#19565);
#16992=AXIS2_PLACEMENT_3D('',#26893,#19567,#19568);
#16993=AXIS2_PLACEMENT_3D('',#26895,#19569,#19570);
#16994=AXIS2_PLACEMENT_3D('',#27085,#19573,#19574);
#16995=AXIS2_PLACEMENT_3D('',#27087,#19575,#19576);
#16996=AXIS2_PLACEMENT_3D('',#27090,#19578,#19579);
#16997=AXIS2_PLACEMENT_3D('',#27092,#19580,#19581);
#16998=AXIS2_PLACEMENT_3D('',#27093,#19582,#19583);
#16999=AXIS2_PLACEMENT_3D('',#27094,#19584,#19585);
#17000=AXIS2_PLACEMENT_3D('',#27128,#19587,#19588);
#17001=AXIS2_PLACEMENT_3D('',#27134,#19589,#19590);
#17002=AXIS2_PLACEMENT_3D('',#27138,#19591,#19592);
#17003=AXIS2_PLACEMENT_3D('',#27140,#19593,#19594);
#17004=AXIS2_PLACEMENT_3D('',#27142,#19596,#19597);
#17005=AXIS2_PLACEMENT_3D('',#27144,#19598,#19599);
#17006=AXIS2_PLACEMENT_3D('',#27288,#19602,#19603);
#17007=AXIS2_PLACEMENT_3D('',#27290,#19604,#19605);
#17008=AXIS2_PLACEMENT_3D('',#27293,#19607,#19608);
#17009=AXIS2_PLACEMENT_3D('',#27294,#19609,#19610);
#17010=AXIS2_PLACEMENT_3D('',#27297,#19612,#19613);
#17011=AXIS2_PLACEMENT_3D('',#27298,#19614,#19615);
#17012=AXIS2_PLACEMENT_3D('',#27300,#19616,#19617);
#17013=AXIS2_PLACEMENT_3D('',#27301,#19618,#19619);
#17014=AXIS2_PLACEMENT_3D('',#27310,#19624,#19625);
#17015=AXIS2_PLACEMENT_3D('',#27316,#19629,#19630);
#17016=AXIS2_PLACEMENT_3D('',#27319,#19633,#19634);
#17017=AXIS2_PLACEMENT_3D('',#27322,#19637,#19638);
#17018=AXIS2_PLACEMENT_3D('',#27328,#19642,#19643);
#17019=AXIS2_PLACEMENT_3D('',#27329,#19644,#19645);
#17020=AXIS2_PLACEMENT_3D('',#27342,#19652,#19653);
#17021=AXIS2_PLACEMENT_3D('',#27352,#19659,#19660);
#17022=AXIS2_PLACEMENT_3D('',#27360,#19665,#19666);
#17023=AXIS2_PLACEMENT_3D('',#27364,#19669,#19670);
#17024=AXIS2_PLACEMENT_3D('',#27370,#19674,#19675);
#17025=AXIS2_PLACEMENT_3D('',#27379,#19681,#19682);
#17026=AXIS2_PLACEMENT_3D('',#27384,#19686,#19687);
#17027=AXIS2_PLACEMENT_3D('',#27386,#19689,#19690);
#17028=AXIS2_PLACEMENT_3D('',#27394,#19695,#19696);
#17029=AXIS2_PLACEMENT_3D('',#27398,#19699,#19700);
#17030=AXIS2_PLACEMENT_3D('',#27410,#19707,#19708);
#17031=AXIS2_PLACEMENT_3D('',#27414,#19710,#19711);
#17032=AXIS2_PLACEMENT_3D('',#27418,#19714,#19715);
#17033=AXIS2_PLACEMENT_3D('',#27422,#19718,#19719);
#17034=AXIS2_PLACEMENT_3D('',#27425,#19722,#19723);
#17035=AXIS2_PLACEMENT_3D('',#27431,#19727,#19728);
#17036=AXIS2_PLACEMENT_3D('',#27440,#19733,#19734);
#17037=AXIS2_PLACEMENT_3D('',#27449,#19739,#19740);
#17038=AXIS2_PLACEMENT_3D('',#27456,#19745,#19746);
#17039=AXIS2_PLACEMENT_3D('',#27463,#19751,#19752);
#17040=AXIS2_PLACEMENT_3D('',#27467,#19755,#19756);
#17041=AXIS2_PLACEMENT_3D('',#27471,#19759,#19760);
#17042=AXIS2_PLACEMENT_3D('',#27475,#19763,#19764);
#17043=AXIS2_PLACEMENT_3D('',#27477,#19765,#19766);
#17044=AXIS2_PLACEMENT_3D('',#27479,#19767,#19768);
#17045=AXIS2_PLACEMENT_3D('',#27481,#19769,#19770);
#17046=AXIS2_PLACEMENT_3D('',#27482,#19771,#19772);
#17047=AXIS2_PLACEMENT_3D('',#27485,#19774,#19775);
#17048=AXIS2_PLACEMENT_3D('',#27486,#19776,#19777);
#17049=AXIS2_PLACEMENT_3D('',#27489,#19779,#19780);
#17050=AXIS2_PLACEMENT_3D('',#27492,#19782,#19783);
#17051=AXIS2_PLACEMENT_3D('',#27493,#19784,#19785);
#17052=AXIS2_PLACEMENT_3D('',#27496,#19787,#19788);
#17053=AXIS2_PLACEMENT_3D('',#27497,#19789,#19790);
#17054=AXIS2_PLACEMENT_3D('',#27500,#19792,#19793);
#17055=AXIS2_PLACEMENT_3D('',#27501,#19794,#19795);
#17056=AXIS2_PLACEMENT_3D('',#27504,#19797,#19798);
#17057=AXIS2_PLACEMENT_3D('',#27505,#19799,#19800);
#17058=AXIS2_PLACEMENT_3D('',#27506,#19801,#19802);
#17059=AXIS2_PLACEMENT_3D('',#27507,#19803,#19804);
#17060=AXIS2_PLACEMENT_3D('',#27508,#19805,#19806);
#17061=AXIS2_PLACEMENT_3D('',#27509,#19807,#19808);
#17062=AXIS2_PLACEMENT_3D('',#27510,#19809,#19810);
#17063=AXIS2_PLACEMENT_3D('',#27511,#19811,#19812);
#17064=AXIS2_PLACEMENT_3D('',#27512,#19813,#19814);
#17065=AXIS2_PLACEMENT_3D('',#27514,#19815,#19816);
#17066=AXIS2_PLACEMENT_3D('',#27516,#19818,#19819);
#17067=AXIS2_PLACEMENT_3D('',#27519,#19821,#19822);
#17068=AXIS2_PLACEMENT_3D('',#27520,#19823,#19824);
#17069=AXIS2_PLACEMENT_3D('',#27522,#19825,#19826);
#17070=AXIS2_PLACEMENT_3D('',#27524,#19828,#19829);
#17071=AXIS2_PLACEMENT_3D('',#27534,#19834,#19835);
#17072=AXIS2_PLACEMENT_3D('',#27536,#19836,#19837);
#17073=AXIS2_PLACEMENT_3D('',#27537,#19838,#19839);
#17074=AXIS2_PLACEMENT_3D('',#27539,#19841,#19842);
#17075=AXIS2_PLACEMENT_3D('',#27543,#19846,#19847);
#17076=AXIS2_PLACEMENT_3D('',#27547,#19851,#19852);
#17077=AXIS2_PLACEMENT_3D('',#27548,#19853,#19854);
#17078=AXIS2_PLACEMENT_3D('',#27549,#19855,#19856);
#17079=AXIS2_PLACEMENT_3D('',#27552,#19859,#19860);
#17080=AXIS2_PLACEMENT_3D('',#27555,#19862,#19863);
#17081=AXIS2_PLACEMENT_3D('',#27556,#19864,#19865);
#17082=AXIS2_PLACEMENT_3D('',#27558,#19866,#19867);
#17083=AXIS2_PLACEMENT_3D('',#27560,#19869,#19870);
#17084=AXIS2_PLACEMENT_3D('',#27562,#19871,#19872);
#17085=AXIS2_PLACEMENT_3D('',#27564,#19874,#19875);
#17086=AXIS2_PLACEMENT_3D('',#27567,#19877,#19878);
#17087=AXIS2_PLACEMENT_3D('',#27568,#19879,#19880);
#17088=AXIS2_PLACEMENT_3D('',#27570,#19882,#19883);
#17089=AXIS2_PLACEMENT_3D('',#27572,#19885,#19886);
#17090=AXIS2_PLACEMENT_3D('',#27573,#19887,#19888);
#17091=AXIS2_PLACEMENT_3D('',#27575,#19890,#19891);
#17092=AXIS2_PLACEMENT_3D('',#27576,#19892,#19893);
#17093=AXIS2_PLACEMENT_3D('',#27577,#19894,#19895);
#17094=AXIS2_PLACEMENT_3D('',#27579,#19897,#19898);
#17095=AXIS2_PLACEMENT_3D('',#27580,#19899,#19900);
#17096=AXIS2_PLACEMENT_3D('',#27581,#19901,#19902);
#17097=AXIS2_PLACEMENT_3D('',#27583,#19904,#19905);
#17098=AXIS2_PLACEMENT_3D('',#27584,#19906,#19907);
#17099=AXIS2_PLACEMENT_3D('',#27585,#19908,#19909);
#17100=AXIS2_PLACEMENT_3D('',#27601,#19911,#19912);
#17101=AXIS2_PLACEMENT_3D('',#27609,#19913,#19914);
#17102=AXIS2_PLACEMENT_3D('',#27657,#19916,#19917);
#17103=AXIS2_PLACEMENT_3D('',#27705,#19919,#19920);
#17104=AXIS2_PLACEMENT_3D('',#27759,#19922,#19923);
#17105=AXIS2_PLACEMENT_3D('',#27807,#19925,#19926);
#17106=AXIS2_PLACEMENT_3D('',#27855,#19928,#19929);
#17107=AXIS2_PLACEMENT_3D('',#27903,#19931,#19932);
#17108=AXIS2_PLACEMENT_3D('',#27954,#19934,#19935);
#17109=AXIS2_PLACEMENT_3D('',#28002,#19937,#19938);
#17110=AXIS2_PLACEMENT_3D('',#28050,#19940,#19941);
#17111=AXIS2_PLACEMENT_3D('',#28104,#19943,#19944);
#17112=AXIS2_PLACEMENT_3D('',#28152,#19946,#19947);
#17113=AXIS2_PLACEMENT_3D('',#28200,#19949,#19950);
#17114=AXIS2_PLACEMENT_3D('',#28254,#19952,#19953);
#17115=AXIS2_PLACEMENT_3D('',#28302,#19955,#19956);
#17116=AXIS2_PLACEMENT_3D('',#28350,#19958,#19959);
#17117=AXIS2_PLACEMENT_3D('',#28404,#19961,#19962);
#17118=AXIS2_PLACEMENT_3D('',#28452,#19964,#19965);
#17119=AXIS2_PLACEMENT_3D('',#28500,#19967,#19968);
#17120=AXIS2_PLACEMENT_3D('',#28554,#19970,#19971);
#17121=AXIS2_PLACEMENT_3D('',#28602,#19973,#19974);
#17122=AXIS2_PLACEMENT_3D('',#28650,#19976,#19977);
#17123=AXIS2_PLACEMENT_3D('',#28701,#19979,#19980);
#17124=AXIS2_PLACEMENT_3D('',#28706,#19982,#19983);
#17125=AXIS2_PLACEMENT_3D('',#28751,#19984,#19985);
#17126=AXIS2_PLACEMENT_3D('',#28765,#19987,#19988);
#17127=AXIS2_PLACEMENT_3D('',#28772,#19989,#19990);
#17128=AXIS2_PLACEMENT_3D('',#28796,#19992,#19993);
#17129=AXIS2_PLACEMENT_3D('',#28821,#19995,#19996);
#17130=AXIS2_PLACEMENT_3D('',#28845,#19998,#19999);
#17131=AXIS2_PLACEMENT_3D('',#28870,#20001,#20002);
#17132=AXIS2_PLACEMENT_3D('',#28895,#20004,#20005);
#17133=AXIS2_PLACEMENT_3D('',#28919,#20007,#20008);
#17134=AXIS2_PLACEMENT_3D('',#28944,#20010,#20011);
#17135=AXIS2_PLACEMENT_3D('',#28969,#20013,#20014);
#17136=AXIS2_PLACEMENT_3D('',#28993,#20016,#20017);
#17137=AXIS2_PLACEMENT_3D('',#29018,#20019,#20020);
#17138=AXIS2_PLACEMENT_3D('',#29043,#20022,#20023);
#17139=AXIS2_PLACEMENT_3D('',#29067,#20025,#20026);
#17140=AXIS2_PLACEMENT_3D('',#29092,#20028,#20029);
#17141=AXIS2_PLACEMENT_3D('',#29117,#20031,#20032);
#17142=AXIS2_PLACEMENT_3D('',#29141,#20034,#20035);
#17143=AXIS2_PLACEMENT_3D('',#29166,#20037,#20038);
#17144=AXIS2_PLACEMENT_3D('',#29190,#20040,#20041);
#17145=AXIS2_PLACEMENT_3D('',#29215,#20043,#20044);
#17146=AXIS2_PLACEMENT_3D('',#29239,#20046,#20047);
#17147=AXIS2_PLACEMENT_3D('',#29264,#20049,#20050);
#17148=AXIS2_PLACEMENT_3D('',#29289,#20052,#20053);
#17149=AXIS2_PLACEMENT_3D('',#29313,#20055,#20056);
#17150=AXIS2_PLACEMENT_3D('',#29322,#20061,#20062);
#17151=AXIS2_PLACEMENT_3D('',#29328,#20066,#20067);
#17152=AXIS2_PLACEMENT_3D('',#29334,#20071,#20072);
#17153=AXIS2_PLACEMENT_3D('',#29337,#20075,#20076);
#17154=AXIS2_PLACEMENT_3D('',#29338,#20077,#20078);
#17155=AXIS2_PLACEMENT_3D('',#29340,#20079,#20080);
#17156=AXIS2_PLACEMENT_3D('',#29343,#20082,#20083);
#17157=AXIS2_PLACEMENT_3D('',#29344,#20084,#20085);
#17158=AXIS2_PLACEMENT_3D('',#30078,#20086,#20087);
#17159=AXIS2_PLACEMENT_3D('',#30080,#20088,#20089);
#17160=AXIS2_PLACEMENT_3D('',#30081,#20090,#20091);
#17161=AXIS2_PLACEMENT_3D('',#30138,#20092,#20093);
#17162=AXIS2_PLACEMENT_3D('',#30139,#20094,#20095);
#17163=AXIS2_PLACEMENT_3D('',#30811,#20096,#20097);
#17164=AXIS2_PLACEMENT_3D('',#30824,#20100,#20101);
#17165=AXIS2_PLACEMENT_3D('',#30834,#20103,#20104);
#17166=AXIS2_PLACEMENT_3D('',#30847,#20107,#20108);
#17167=AXIS2_PLACEMENT_3D('',#30857,#20110,#20111);
#17168=AXIS2_PLACEMENT_3D('',#30870,#20114,#20115);
#17169=AXIS2_PLACEMENT_3D('',#30880,#20117,#20118);
#17170=AXIS2_PLACEMENT_3D('',#30893,#20121,#20122);
#17171=AXIS2_PLACEMENT_3D('',#30903,#20124,#20125);
#17172=AXIS2_PLACEMENT_3D('',#30916,#20128,#20129);
#17173=AXIS2_PLACEMENT_3D('',#30926,#20131,#20132);
#17174=AXIS2_PLACEMENT_3D('',#30939,#20135,#20136);
#17175=AXIS2_PLACEMENT_3D('',#30949,#20138,#20139);
#17176=AXIS2_PLACEMENT_3D('',#30962,#20142,#20143);
#17177=AXIS2_PLACEMENT_3D('',#30972,#20145,#20146);
#17178=AXIS2_PLACEMENT_3D('',#30985,#20149,#20150);
#17179=AXIS2_PLACEMENT_3D('',#30995,#20152,#20153);
#17180=AXIS2_PLACEMENT_3D('',#31008,#20156,#20157);
#17181=AXIS2_PLACEMENT_3D('',#31018,#20159,#20160);
#17182=AXIS2_PLACEMENT_3D('',#31031,#20163,#20164);
#17183=AXIS2_PLACEMENT_3D('',#31041,#20166,#20167);
#17184=AXIS2_PLACEMENT_3D('',#31054,#20170,#20171);
#17185=AXIS2_PLACEMENT_3D('',#31064,#20173,#20174);
#17186=AXIS2_PLACEMENT_3D('',#31077,#20177,#20178);
#17187=AXIS2_PLACEMENT_3D('',#31087,#20180,#20181);
#17188=AXIS2_PLACEMENT_3D('',#31100,#20184,#20185);
#17189=AXIS2_PLACEMENT_3D('',#31110,#20187,#20188);
#17190=AXIS2_PLACEMENT_3D('',#31123,#20191,#20192);
#17191=AXIS2_PLACEMENT_3D('',#31133,#20194,#20195);
#17192=AXIS2_PLACEMENT_3D('',#31146,#20198,#20199);
#17193=AXIS2_PLACEMENT_3D('',#31156,#20201,#20202);
#17194=AXIS2_PLACEMENT_3D('',#31169,#20205,#20206);
#17195=AXIS2_PLACEMENT_3D('',#31179,#20208,#20209);
#17196=AXIS2_PLACEMENT_3D('',#31192,#20212,#20213);
#17197=AXIS2_PLACEMENT_3D('',#31202,#20215,#20216);
#17198=AXIS2_PLACEMENT_3D('',#31215,#20219,#20220);
#17199=AXIS2_PLACEMENT_3D('',#31225,#20222,#20223);
#17200=AXIS2_PLACEMENT_3D('',#31238,#20226,#20227);
#17201=AXIS2_PLACEMENT_3D('',#31248,#20229,#20230);
#17202=AXIS2_PLACEMENT_3D('',#31261,#20233,#20234);
#17203=AXIS2_PLACEMENT_3D('',#31271,#20236,#20237);
#17204=AXIS2_PLACEMENT_3D('',#31284,#20240,#20241);
#17205=AXIS2_PLACEMENT_3D('',#31294,#20243,#20244);
#17206=AXIS2_PLACEMENT_3D('',#31307,#20247,#20248);
#17207=AXIS2_PLACEMENT_3D('',#31317,#20250,#20251);
#17208=AXIS2_PLACEMENT_3D('',#31330,#20254,#20255);
#17209=AXIS2_PLACEMENT_3D('',#31340,#20257,#20258);
#17210=AXIS2_PLACEMENT_3D('',#31353,#20261,#20262);
#17211=AXIS2_PLACEMENT_3D('',#31363,#20264,#20265);
#17212=AXIS2_PLACEMENT_3D('',#31376,#20268,#20269);
#17213=AXIS2_PLACEMENT_3D('',#31386,#20271,#20272);
#17214=AXIS2_PLACEMENT_3D('',#31399,#20275,#20276);
#17215=AXIS2_PLACEMENT_3D('',#31409,#20278,#20279);
#17216=AXIS2_PLACEMENT_3D('',#31422,#20282,#20283);
#17217=AXIS2_PLACEMENT_3D('',#31432,#20285,#20286);
#17218=AXIS2_PLACEMENT_3D('',#31445,#20289,#20290);
#17219=AXIS2_PLACEMENT_3D('',#31455,#20292,#20293);
#17220=AXIS2_PLACEMENT_3D('',#31468,#20296,#20297);
#17221=AXIS2_PLACEMENT_3D('',#31478,#20299,#20300);
#17222=AXIS2_PLACEMENT_3D('',#31491,#20303,#20304);
#17223=AXIS2_PLACEMENT_3D('',#31501,#20306,#20307);
#17224=AXIS2_PLACEMENT_3D('',#31502,#20308,#20309);
#17225=AXIS2_PLACEMENT_3D('',#31503,#20310,#20311);
#17226=AXIS2_PLACEMENT_3D('',#31504,#20312,#20313);
#17227=AXIS2_PLACEMENT_3D('',#31505,#20314,#20315);
#17228=AXIS2_PLACEMENT_3D('',#31506,#20316,#20317);
#17229=AXIS2_PLACEMENT_3D('',#31507,#20318,#20319);
#17230=AXIS2_PLACEMENT_3D('',#31508,#20320,#20321);
#17231=AXIS2_PLACEMENT_3D('',#31509,#20322,#20323);
#17232=AXIS2_PLACEMENT_3D('',#31510,#20324,#20325);
#17233=AXIS2_PLACEMENT_3D('',#31511,#20326,#20327);
#17234=AXIS2_PLACEMENT_3D('',#31512,#20328,#20329);
#17235=AXIS2_PLACEMENT_3D('',#31513,#20330,#20331);
#17236=AXIS2_PLACEMENT_3D('',#31514,#20332,#20333);
#17237=AXIS2_PLACEMENT_3D('',#31515,#20334,#20335);
#17238=AXIS2_PLACEMENT_3D('',#31516,#20336,#20337);
#17239=AXIS2_PLACEMENT_3D('',#31517,#20338,#20339);
#17240=AXIS2_PLACEMENT_3D('',#31518,#20340,#20341);
#17241=AXIS2_PLACEMENT_3D('',#31519,#20342,#20343);
#17242=AXIS2_PLACEMENT_3D('',#31520,#20344,#20345);
#17243=AXIS2_PLACEMENT_3D('',#31521,#20346,#20347);
#17244=AXIS2_PLACEMENT_3D('',#31522,#20348,#20349);
#17245=AXIS2_PLACEMENT_3D('',#31523,#20350,#20351);
#17246=AXIS2_PLACEMENT_3D('',#31524,#20352,#20353);
#17247=AXIS2_PLACEMENT_3D('',#31525,#20354,#20355);
#17248=AXIS2_PLACEMENT_3D('',#31526,#20356,#20357);
#17249=AXIS2_PLACEMENT_3D('',#31527,#20358,#20359);
#17250=AXIS2_PLACEMENT_3D('',#31528,#20360,#20361);
#17251=AXIS2_PLACEMENT_3D('',#31529,#20362,#20363);
#17252=AXIS2_PLACEMENT_3D('',#31530,#20364,#20365);
#17253=AXIS2_PLACEMENT_3D('',#31531,#20366,#20367);
#17254=AXIS2_PLACEMENT_3D('',#31532,#20368,#20369);
#17255=AXIS2_PLACEMENT_3D('',#31533,#20370,#20371);
#17256=AXIS2_PLACEMENT_3D('',#31534,#20372,#20373);
#17257=AXIS2_PLACEMENT_3D('',#31535,#20374,#20375);
#17258=AXIS2_PLACEMENT_3D('',#31536,#20376,#20377);
#17259=AXIS2_PLACEMENT_3D('',#31537,#20378,#20379);
#17260=AXIS2_PLACEMENT_3D('',#31538,#20380,#20381);
#17261=AXIS2_PLACEMENT_3D('',#31539,#20382,#20383);
#17262=AXIS2_PLACEMENT_3D('',#31540,#20384,#20385);
#17263=AXIS2_PLACEMENT_3D('',#31541,#20386,#20387);
#17264=AXIS2_PLACEMENT_3D('',#31542,#20388,#20389);
#17265=AXIS2_PLACEMENT_3D('',#31543,#20390,#20391);
#17266=AXIS2_PLACEMENT_3D('',#31544,#20392,#20393);
#17267=AXIS2_PLACEMENT_3D('',#31545,#20394,#20395);
#17268=AXIS2_PLACEMENT_3D('',#31546,#20396,#20397);
#17269=AXIS2_PLACEMENT_3D('',#31547,#20398,#20399);
#17270=AXIS2_PLACEMENT_3D('',#31548,#20400,#20401);
#17271=AXIS2_PLACEMENT_3D('',#31549,#20402,#20403);
#17272=AXIS2_PLACEMENT_3D('',#31550,#20404,#20405);
#17273=AXIS2_PLACEMENT_3D('',#31551,#20406,#20407);
#17274=AXIS2_PLACEMENT_3D('',#31552,#20408,#20409);
#17275=AXIS2_PLACEMENT_3D('',#31553,#20410,#20411);
#17276=AXIS2_PLACEMENT_3D('',#31554,#20412,#20413);
#17277=AXIS2_PLACEMENT_3D('',#31555,#20414,#20415);
#17278=AXIS2_PLACEMENT_3D('',#31556,#20416,#20417);
#17279=AXIS2_PLACEMENT_3D('',#31557,#20418,#20419);
#17280=AXIS2_PLACEMENT_3D('',#31558,#20420,#20421);
#17281=AXIS2_PLACEMENT_3D('',#31559,#20422,#20423);
#17282=AXIS2_PLACEMENT_3D('',#31560,#20424,#20425);
#17283=AXIS2_PLACEMENT_3D('',#31561,#20426,#20427);
#17284=AXIS2_PLACEMENT_3D('',#31562,#20428,#20429);
#17285=AXIS2_PLACEMENT_3D('',#31563,#20430,#20431);
#17286=AXIS2_PLACEMENT_3D('',#31564,#20432,#20433);
#17287=AXIS2_PLACEMENT_3D('',#31565,#20434,#20435);
#17288=AXIS2_PLACEMENT_3D('',#31566,#20436,#20437);
#17289=AXIS2_PLACEMENT_3D('',#31567,#20438,#20439);
#17290=AXIS2_PLACEMENT_3D('',#31568,#20440,#20441);
#17291=AXIS2_PLACEMENT_3D('',#31569,#20442,#20443);
#17292=AXIS2_PLACEMENT_3D('',#31570,#20444,#20445);
#17293=AXIS2_PLACEMENT_3D('',#31571,#20446,#20447);
#17294=AXIS2_PLACEMENT_3D('',#31572,#20448,#20449);
#17295=AXIS2_PLACEMENT_3D('',#31573,#20450,#20451);
#17296=AXIS2_PLACEMENT_3D('',#31574,#20452,#20453);
#17297=AXIS2_PLACEMENT_3D('',#31575,#20454,#20455);
#17298=AXIS2_PLACEMENT_3D('',#31576,#20456,#20457);
#17299=AXIS2_PLACEMENT_3D('',#31577,#20458,#20459);
#17300=AXIS2_PLACEMENT_3D('',#31578,#20460,#20461);
#17301=AXIS2_PLACEMENT_3D('',#31579,#20462,#20463);
#17302=AXIS2_PLACEMENT_3D('',#31580,#20464,#20465);
#17303=AXIS2_PLACEMENT_3D('',#31581,#20466,#20467);
#17304=AXIS2_PLACEMENT_3D('',#31582,#20468,#20469);
#17305=AXIS2_PLACEMENT_3D('',#31583,#20470,#20471);
#17306=AXIS2_PLACEMENT_3D('',#31584,#20472,#20473);
#17307=AXIS2_PLACEMENT_3D('',#31585,#20474,#20475);
#17308=AXIS2_PLACEMENT_3D('',#31586,#20476,#20477);
#17309=AXIS2_PLACEMENT_3D('',#31587,#20478,#20479);
#17310=AXIS2_PLACEMENT_3D('',#31588,#20480,#20481);
#17311=AXIS2_PLACEMENT_3D('',#31589,#20482,#20483);
#17312=AXIS2_PLACEMENT_3D('',#31590,#20484,#20485);
#17313=AXIS2_PLACEMENT_3D('',#31591,#20486,#20487);
#17314=AXIS2_PLACEMENT_3D('',#31594,#20489,#20490);
#17315=AXIS2_PLACEMENT_3D('',#31595,#20491,#20492);
#17316=AXIS2_PLACEMENT_3D('',#31597,#20493,#20494);
#17317=AXIS2_PLACEMENT_3D('',#31598,#20495,#20496);
#17318=AXIS2_PLACEMENT_3D('',#31600,#20498,#20499);
#17319=AXIS2_PLACEMENT_3D('',#31601,#20500,#20501);
#17320=AXIS2_PLACEMENT_3D('',#31602,#20502,#20503);
#17321=AXIS2_PLACEMENT_3D('',#31603,#20504,#20505);
#17322=AXIS2_PLACEMENT_3D('',#31605,#20506,#20507);
#17323=AXIS2_PLACEMENT_3D('',#31607,#20509,#20510);
#17324=AXIS2_PLACEMENT_3D('',#31608,#20511,#20512);
#17325=AXIS2_PLACEMENT_3D('',#31609,#20513,#20514);
#17326=AXIS2_PLACEMENT_3D('',#31612,#20515,#20516);
#17327=AXIS2_PLACEMENT_3D('',#31613,#20517,#20518);
#17328=AXIS2_PLACEMENT_3D('',#32209,#20519,#20520);
#17329=AXIS2_PLACEMENT_3D('',#32265,#20521,#20522);
#17330=AXIS2_PLACEMENT_3D('',#32266,#20523,#20524);
#17331=AXIS2_PLACEMENT_3D('',#32267,#20525,#20526);
#17332=AXIS2_PLACEMENT_3D('',#32268,#20527,#20528);
#17333=AXIS2_PLACEMENT_3D('',#32269,#20529,#20530);
#17334=AXIS2_PLACEMENT_3D('',#32285,#20532,#20533);
#17335=AXIS2_PLACEMENT_3D('',#32293,#20534,#20535);
#17336=AXIS2_PLACEMENT_3D('',#32341,#20537,#20538);
#17337=AXIS2_PLACEMENT_3D('',#32389,#20540,#20541);
#17338=AXIS2_PLACEMENT_3D('',#32440,#20543,#20544);
#17339=AXIS2_PLACEMENT_3D('',#32491,#20546,#20547);
#17340=AXIS2_PLACEMENT_3D('',#32539,#20549,#20550);
#17341=AXIS2_PLACEMENT_3D('',#32587,#20552,#20553);
#17342=AXIS2_PLACEMENT_3D('',#32641,#20555,#20556);
#17343=AXIS2_PLACEMENT_3D('',#32689,#20558,#20559);
#17344=AXIS2_PLACEMENT_3D('',#32737,#20561,#20562);
#17345=AXIS2_PLACEMENT_3D('',#32791,#20564,#20565);
#17346=AXIS2_PLACEMENT_3D('',#32839,#20567,#20568);
#17347=AXIS2_PLACEMENT_3D('',#32887,#20570,#20571);
#17348=AXIS2_PLACEMENT_3D('',#32935,#20573,#20574);
#17349=AXIS2_PLACEMENT_3D('',#32989,#20576,#20577);
#17350=AXIS2_PLACEMENT_3D('',#33037,#20579,#20580);
#17351=AXIS2_PLACEMENT_3D('',#33085,#20582,#20583);
#17352=AXIS2_PLACEMENT_3D('',#33139,#20585,#20586);
#17353=AXIS2_PLACEMENT_3D('',#33187,#20588,#20589);
#17354=AXIS2_PLACEMENT_3D('',#33235,#20591,#20592);
#17355=AXIS2_PLACEMENT_3D('',#33289,#20594,#20595);
#17356=AXIS2_PLACEMENT_3D('',#33337,#20597,#20598);
#17357=AXIS2_PLACEMENT_3D('',#33349,#20600,#20601);
#17358=AXIS2_PLACEMENT_3D('',#33355,#20602,#20603);
#17359=AXIS2_PLACEMENT_3D('',#33379,#20605,#20606);
#17360=AXIS2_PLACEMENT_3D('',#33404,#20608,#20609);
#17361=AXIS2_PLACEMENT_3D('',#33429,#20611,#20612);
#17362=AXIS2_PLACEMENT_3D('',#33453,#20614,#20615);
#17363=AXIS2_PLACEMENT_3D('',#33478,#20617,#20618);
#17364=AXIS2_PLACEMENT_3D('',#33503,#20620,#20621);
#17365=AXIS2_PLACEMENT_3D('',#33527,#20623,#20624);
#17366=AXIS2_PLACEMENT_3D('',#33552,#20626,#20627);
#17367=AXIS2_PLACEMENT_3D('',#33577,#20629,#20630);
#17368=AXIS2_PLACEMENT_3D('',#33601,#20632,#20633);
#17369=AXIS2_PLACEMENT_3D('',#33625,#20635,#20636);
#17370=AXIS2_PLACEMENT_3D('',#33650,#20638,#20639);
#17371=AXIS2_PLACEMENT_3D('',#33675,#20641,#20642);
#17372=AXIS2_PLACEMENT_3D('',#33699,#20644,#20645);
#17373=AXIS2_PLACEMENT_3D('',#33724,#20647,#20648);
#17374=AXIS2_PLACEMENT_3D('',#33749,#20650,#20651);
#17375=AXIS2_PLACEMENT_3D('',#33773,#20653,#20654);
#17376=AXIS2_PLACEMENT_3D('',#33798,#20656,#20657);
#17377=AXIS2_PLACEMENT_3D('',#33822,#20659,#20660);
#17378=AXIS2_PLACEMENT_3D('',#33847,#20662,#20663);
#17379=AXIS2_PLACEMENT_3D('',#33871,#20665,#20666);
#17380=AXIS2_PLACEMENT_3D('',#33926,#20667,#20668);
#17381=AXIS2_PLACEMENT_3D('',#33928,#20669,#20670);
#17382=AXIS2_PLACEMENT_3D('',#34638,#20671,#20672);
#17383=AXIS2_PLACEMENT_3D('',#34640,#20673,#20674);
#17384=AXIS2_PLACEMENT_3D('',#34641,#20675,#20676);
#17385=AXIS2_PLACEMENT_3D('',#34695,#20677,#20678);
#17386=AXIS2_PLACEMENT_3D('',#34696,#20679,#20680);
#17387=AXIS2_PLACEMENT_3D('',#35297,#20681,#20682);
#17388=AXIS2_PLACEMENT_3D('',#35299,#20683,#20684);
#17389=AXIS2_PLACEMENT_3D('',#35300,#20685,#20686);
#17390=AXIS2_PLACEMENT_3D('',#35301,#20687,#20688);
#17391=AXIS2_PLACEMENT_3D('',#35302,#20689,#20690);
#17392=AXIS2_PLACEMENT_3D('',#35303,#20691,#20692);
#17393=AXIS2_PLACEMENT_3D('',#35310,#20695,#20696);
#17394=AXIS2_PLACEMENT_3D('',#35316,#20699,#20700);
#17395=AXIS2_PLACEMENT_3D('',#35322,#20703,#20704);
#17396=AXIS2_PLACEMENT_3D('',#35328,#20707,#20708);
#17397=AXIS2_PLACEMENT_3D('',#35334,#20711,#20712);
#17398=AXIS2_PLACEMENT_3D('',#35340,#20715,#20716);
#17399=AXIS2_PLACEMENT_3D('',#35346,#20719,#20720);
#17400=AXIS2_PLACEMENT_3D('',#35352,#20723,#20724);
#17401=AXIS2_PLACEMENT_3D('',#35358,#20727,#20728);
#17402=AXIS2_PLACEMENT_3D('',#35364,#20731,#20732);
#17403=AXIS2_PLACEMENT_3D('',#35370,#20735,#20736);
#17404=AXIS2_PLACEMENT_3D('',#35376,#20739,#20740);
#17405=AXIS2_PLACEMENT_3D('',#35382,#20743,#20744);
#17406=AXIS2_PLACEMENT_3D('',#35388,#20747,#20748);
#17407=AXIS2_PLACEMENT_3D('',#35394,#20751,#20752);
#17408=AXIS2_PLACEMENT_3D('',#35400,#20755,#20756);
#17409=AXIS2_PLACEMENT_3D('',#35406,#20759,#20760);
#17410=AXIS2_PLACEMENT_3D('',#35412,#20763,#20764);
#17411=AXIS2_PLACEMENT_3D('',#35418,#20767,#20768);
#17412=AXIS2_PLACEMENT_3D('',#35424,#20771,#20772);
#17413=AXIS2_PLACEMENT_3D('',#35430,#20775,#20776);
#17414=AXIS2_PLACEMENT_3D('',#35436,#20779,#20780);
#17415=AXIS2_PLACEMENT_3D('',#35442,#20783,#20784);
#17416=AXIS2_PLACEMENT_3D('',#35448,#20787,#20788);
#17417=AXIS2_PLACEMENT_3D('',#35454,#20791,#20792);
#17418=AXIS2_PLACEMENT_3D('',#35460,#20795,#20796);
#17419=AXIS2_PLACEMENT_3D('',#35466,#20799,#20800);
#17420=AXIS2_PLACEMENT_3D('',#35472,#20803,#20804);
#17421=AXIS2_PLACEMENT_3D('',#35478,#20807,#20808);
#17422=AXIS2_PLACEMENT_3D('',#35484,#20811,#20812);
#17423=AXIS2_PLACEMENT_3D('',#35490,#20815,#20816);
#17424=AXIS2_PLACEMENT_3D('',#35496,#20819,#20820);
#17425=AXIS2_PLACEMENT_3D('',#35502,#20823,#20824);
#17426=AXIS2_PLACEMENT_3D('',#35508,#20827,#20828);
#17427=AXIS2_PLACEMENT_3D('',#35514,#20831,#20832);
#17428=AXIS2_PLACEMENT_3D('',#35519,#20835,#20836);
#17429=AXIS2_PLACEMENT_3D('',#35520,#20837,#20838);
#17430=AXIS2_PLACEMENT_3D('',#35524,#20840,#20841);
#17431=AXIS2_PLACEMENT_3D('',#35525,#20842,#20843);
#17432=AXIS2_PLACEMENT_3D('',#35528,#20845,#20846);
#17433=AXIS2_PLACEMENT_3D('',#35529,#20847,#20848);
#17434=AXIS2_PLACEMENT_3D('',#35532,#20850,#20851);
#17435=AXIS2_PLACEMENT_3D('',#35533,#20852,#20853);
#17436=AXIS2_PLACEMENT_3D('',#35536,#20855,#20856);
#17437=AXIS2_PLACEMENT_3D('',#35537,#20857,#20858);
#17438=AXIS2_PLACEMENT_3D('',#35540,#20860,#20861);
#17439=AXIS2_PLACEMENT_3D('',#35541,#20862,#20863);
#17440=AXIS2_PLACEMENT_3D('',#35543,#20865,#20866);
#17441=AXIS2_PLACEMENT_3D('',#35544,#20867,#20868);
#17442=AXIS2_PLACEMENT_3D('',#35549,#20870,#20871);
#17443=AXIS2_PLACEMENT_3D('',#35558,#20872,#20873);
#17444=AXIS2_PLACEMENT_3D('',#35567,#20874,#20875);
#17445=AXIS2_PLACEMENT_3D('',#35576,#20876,#20877);
#17446=AXIS2_PLACEMENT_3D('',#35585,#20878,#20879);
#17447=AXIS2_PLACEMENT_3D('',#35594,#20880,#20881);
#17448=AXIS2_PLACEMENT_3D('',#35602,#20882,#20883);
#17449=AXIS2_PLACEMENT_3D('',#35603,#20884,#20885);
#17450=AXIS2_PLACEMENT_3D('',#35609,#20889,#20890);
#17451=AXIS2_PLACEMENT_3D('',#35613,#20893,#20894);
#17452=AXIS2_PLACEMENT_3D('',#35617,#20897,#20898);
#17453=AXIS2_PLACEMENT_3D('',#35621,#20901,#20902);
#17454=AXIS2_PLACEMENT_3D('',#35625,#20905,#20906);
#17455=AXIS2_PLACEMENT_3D('',#35629,#20909,#20910);
#17456=AXIS2_PLACEMENT_3D('',#35633,#20913,#20914);
#17457=AXIS2_PLACEMENT_3D('',#35637,#20917,#20918);
#17458=AXIS2_PLACEMENT_3D('',#35641,#20921,#20922);
#17459=AXIS2_PLACEMENT_3D('',#35643,#20924,#20925);
#17460=AXIS2_PLACEMENT_3D('',#35645,#20927,#20928);
#17461=AXIS2_PLACEMENT_3D('',#35646,#20929,#20930);
#17462=AXIS2_PLACEMENT_3D('',#35648,#20932,#20933);
#17463=AXIS2_PLACEMENT_3D('',#35652,#20936,#20937);
#17464=AXIS2_PLACEMENT_3D('',#35654,#20939,#20940);
#17465=AXIS2_PLACEMENT_3D('',#35656,#20942,#20943);
#17466=AXIS2_PLACEMENT_3D('',#35660,#20946,#20947);
#17467=AXIS2_PLACEMENT_3D('',#35662,#20949,#20950);
#17468=AXIS2_PLACEMENT_3D('',#35663,#20951,#20952);
#17469=AXIS2_PLACEMENT_3D('',#35664,#20953,#20954);
#17470=AXIS2_PLACEMENT_3D('',#35666,#20956,#20957);
#17471=AXIS2_PLACEMENT_3D('',#35667,#20958,#20959);
#17472=AXIS2_PLACEMENT_3D('',#35668,#20960,#20961);
#17473=AXIS2_PLACEMENT_3D('',#35669,#20962,#20963);
#17474=AXIS2_PLACEMENT_3D('',#35677,#20966,#20967);
#17475=AXIS2_PLACEMENT_3D('',#35683,#20969,#20970);
#17476=AXIS2_PLACEMENT_3D('',#35691,#20973,#20974);
#17477=AXIS2_PLACEMENT_3D('',#35697,#20976,#20977);
#17478=AXIS2_PLACEMENT_3D('',#35705,#20980,#20981);
#17479=AXIS2_PLACEMENT_3D('',#35711,#20983,#20984);
#17480=AXIS2_PLACEMENT_3D('',#35719,#20987,#20988);
#17481=AXIS2_PLACEMENT_3D('',#35725,#20990,#20991);
#17482=AXIS2_PLACEMENT_3D('',#35733,#20994,#20995);
#17483=AXIS2_PLACEMENT_3D('',#35739,#20997,#20998);
#17484=AXIS2_PLACEMENT_3D('',#35747,#21001,#21002);
#17485=AXIS2_PLACEMENT_3D('',#35753,#21004,#21005);
#17486=AXIS2_PLACEMENT_3D('',#35761,#21008,#21009);
#17487=AXIS2_PLACEMENT_3D('',#35767,#21011,#21012);
#17488=AXIS2_PLACEMENT_3D('',#35775,#21015,#21016);
#17489=AXIS2_PLACEMENT_3D('',#35781,#21018,#21019);
#17490=AXIS2_PLACEMENT_3D('',#35789,#21022,#21023);
#17491=AXIS2_PLACEMENT_3D('',#35795,#21025,#21026);
#17492=AXIS2_PLACEMENT_3D('',#35803,#21029,#21030);
#17493=AXIS2_PLACEMENT_3D('',#35809,#21032,#21033);
#17494=AXIS2_PLACEMENT_3D('',#35817,#21036,#21037);
#17495=AXIS2_PLACEMENT_3D('',#35823,#21039,#21040);
#17496=AXIS2_PLACEMENT_3D('',#35831,#21043,#21044);
#17497=AXIS2_PLACEMENT_3D('',#35837,#21046,#21047);
#17498=AXIS2_PLACEMENT_3D('',#35845,#21050,#21051);
#17499=AXIS2_PLACEMENT_3D('',#35851,#21053,#21054);
#17500=AXIS2_PLACEMENT_3D('',#35859,#21057,#21058);
#17501=AXIS2_PLACEMENT_3D('',#35865,#21060,#21061);
#17502=AXIS2_PLACEMENT_3D('',#35873,#21064,#21065);
#17503=AXIS2_PLACEMENT_3D('',#35879,#21067,#21068);
#17504=AXIS2_PLACEMENT_3D('',#35887,#21071,#21072);
#17505=AXIS2_PLACEMENT_3D('',#35893,#21074,#21075);
#17506=AXIS2_PLACEMENT_3D('',#35901,#21078,#21079);
#17507=AXIS2_PLACEMENT_3D('',#35907,#21081,#21082);
#17508=AXIS2_PLACEMENT_3D('',#35915,#21085,#21086);
#17509=AXIS2_PLACEMENT_3D('',#35921,#21088,#21089);
#17510=AXIS2_PLACEMENT_3D('',#35929,#21092,#21093);
#17511=AXIS2_PLACEMENT_3D('',#35935,#21095,#21096);
#17512=AXIS2_PLACEMENT_3D('',#35943,#21099,#21100);
#17513=AXIS2_PLACEMENT_3D('',#35949,#21102,#21103);
#17514=AXIS2_PLACEMENT_3D('',#35957,#21106,#21107);
#17515=AXIS2_PLACEMENT_3D('',#35963,#21109,#21110);
#17516=AXIS2_PLACEMENT_3D('',#35971,#21113,#21114);
#17517=AXIS2_PLACEMENT_3D('',#35977,#21116,#21117);
#17518=AXIS2_PLACEMENT_3D('',#35985,#21120,#21121);
#17519=AXIS2_PLACEMENT_3D('',#35991,#21123,#21124);
#17520=AXIS2_PLACEMENT_3D('',#35999,#21127,#21128);
#17521=AXIS2_PLACEMENT_3D('',#36005,#21130,#21131);
#17522=AXIS2_PLACEMENT_3D('',#36013,#21134,#21135);
#17523=AXIS2_PLACEMENT_3D('',#36019,#21137,#21138);
#17524=AXIS2_PLACEMENT_3D('',#36027,#21141,#21142);
#17525=AXIS2_PLACEMENT_3D('',#36033,#21144,#21145);
#17526=AXIS2_PLACEMENT_3D('',#36041,#21148,#21149);
#17527=AXIS2_PLACEMENT_3D('',#36047,#21151,#21152);
#17528=AXIS2_PLACEMENT_3D('',#36055,#21155,#21156);
#17529=AXIS2_PLACEMENT_3D('',#36061,#21158,#21159);
#17530=AXIS2_PLACEMENT_3D('',#36069,#21162,#21163);
#17531=AXIS2_PLACEMENT_3D('',#36075,#21165,#21166);
#17532=AXIS2_PLACEMENT_3D('',#36083,#21169,#21170);
#17533=AXIS2_PLACEMENT_3D('',#36089,#21172,#21173);
#17534=AXIS2_PLACEMENT_3D('',#36097,#21176,#21177);
#17535=AXIS2_PLACEMENT_3D('',#36103,#21179,#21180);
#17536=AXIS2_PLACEMENT_3D('',#36111,#21183,#21184);
#17537=AXIS2_PLACEMENT_3D('',#36117,#21186,#21187);
#17538=AXIS2_PLACEMENT_3D('',#36125,#21190,#21191);
#17539=AXIS2_PLACEMENT_3D('',#36131,#21193,#21194);
#17540=AXIS2_PLACEMENT_3D('',#36139,#21197,#21198);
#17541=AXIS2_PLACEMENT_3D('',#36145,#21200,#21201);
#17542=AXIS2_PLACEMENT_3D('',#36153,#21204,#21205);
#17543=AXIS2_PLACEMENT_3D('',#36159,#21207,#21208);
#17544=AXIS2_PLACEMENT_3D('',#36167,#21211,#21212);
#17545=AXIS2_PLACEMENT_3D('',#36173,#21214,#21215);
#17546=AXIS2_PLACEMENT_3D('',#36174,#21216,#21217);
#17547=AXIS2_PLACEMENT_3D('',#36175,#21218,#21219);
#17548=AXIS2_PLACEMENT_3D('',#36176,#21220,#21221);
#17549=AXIS2_PLACEMENT_3D('',#36177,#21222,#21223);
#17550=AXIS2_PLACEMENT_3D('',#36178,#21224,#21225);
#17551=AXIS2_PLACEMENT_3D('',#36179,#21226,#21227);
#17552=AXIS2_PLACEMENT_3D('',#36180,#21228,#21229);
#17553=AXIS2_PLACEMENT_3D('',#36181,#21230,#21231);
#17554=AXIS2_PLACEMENT_3D('',#36182,#21232,#21233);
#17555=AXIS2_PLACEMENT_3D('',#36183,#21234,#21235);
#17556=AXIS2_PLACEMENT_3D('',#36184,#21236,#21237);
#17557=AXIS2_PLACEMENT_3D('',#36185,#21238,#21239);
#17558=AXIS2_PLACEMENT_3D('',#36186,#21240,#21241);
#17559=AXIS2_PLACEMENT_3D('',#36187,#21242,#21243);
#17560=AXIS2_PLACEMENT_3D('',#36188,#21244,#21245);
#17561=AXIS2_PLACEMENT_3D('',#36189,#21246,#21247);
#17562=AXIS2_PLACEMENT_3D('',#36190,#21248,#21249);
#17563=AXIS2_PLACEMENT_3D('',#36191,#21250,#21251);
#17564=AXIS2_PLACEMENT_3D('',#36192,#21252,#21253);
#17565=AXIS2_PLACEMENT_3D('',#36193,#21254,#21255);
#17566=AXIS2_PLACEMENT_3D('',#36194,#21256,#21257);
#17567=AXIS2_PLACEMENT_3D('',#36195,#21258,#21259);
#17568=AXIS2_PLACEMENT_3D('',#36196,#21260,#21261);
#17569=AXIS2_PLACEMENT_3D('',#36197,#21262,#21263);
#17570=AXIS2_PLACEMENT_3D('',#36198,#21264,#21265);
#17571=AXIS2_PLACEMENT_3D('',#36199,#21266,#21267);
#17572=AXIS2_PLACEMENT_3D('',#36200,#21268,#21269);
#17573=AXIS2_PLACEMENT_3D('',#36201,#21270,#21271);
#17574=AXIS2_PLACEMENT_3D('',#36202,#21272,#21273);
#17575=AXIS2_PLACEMENT_3D('',#36203,#21274,#21275);
#17576=AXIS2_PLACEMENT_3D('',#36204,#21276,#21277);
#17577=AXIS2_PLACEMENT_3D('',#36205,#21278,#21279);
#17578=AXIS2_PLACEMENT_3D('',#36206,#21280,#21281);
#17579=AXIS2_PLACEMENT_3D('',#36207,#21282,#21283);
#17580=AXIS2_PLACEMENT_3D('',#36208,#21284,#21285);
#17581=AXIS2_PLACEMENT_3D('',#36209,#21286,#21287);
#17582=AXIS2_PLACEMENT_3D('',#36210,#21288,#21289);
#17583=AXIS2_PLACEMENT_3D('',#36211,#21290,#21291);
#17584=AXIS2_PLACEMENT_3D('',#36212,#21292,#21293);
#17585=AXIS2_PLACEMENT_3D('',#36213,#21294,#21295);
#17586=AXIS2_PLACEMENT_3D('',#36214,#21296,#21297);
#17587=AXIS2_PLACEMENT_3D('',#36215,#21298,#21299);
#17588=AXIS2_PLACEMENT_3D('',#36216,#21300,#21301);
#17589=AXIS2_PLACEMENT_3D('',#36217,#21302,#21303);
#17590=AXIS2_PLACEMENT_3D('',#36218,#21304,#21305);
#17591=AXIS2_PLACEMENT_3D('',#36219,#21306,#21307);
#17592=AXIS2_PLACEMENT_3D('',#36220,#21308,#21309);
#17593=AXIS2_PLACEMENT_3D('',#36221,#21310,#21311);
#17594=AXIS2_PLACEMENT_3D('',#36222,#21312,#21313);
#17595=AXIS2_PLACEMENT_3D('',#36223,#21314,#21315);
#17596=AXIS2_PLACEMENT_3D('',#36224,#21316,#21317);
#17597=AXIS2_PLACEMENT_3D('',#36225,#21318,#21319);
#17598=AXIS2_PLACEMENT_3D('',#36226,#21320,#21321);
#17599=AXIS2_PLACEMENT_3D('',#36227,#21322,#21323);
#17600=AXIS2_PLACEMENT_3D('',#36228,#21324,#21325);
#17601=AXIS2_PLACEMENT_3D('',#36229,#21326,#21327);
#17602=AXIS2_PLACEMENT_3D('',#36230,#21328,#21329);
#17603=AXIS2_PLACEMENT_3D('',#36231,#21330,#21331);
#17604=AXIS2_PLACEMENT_3D('',#36232,#21332,#21333);
#17605=AXIS2_PLACEMENT_3D('',#36233,#21334,#21335);
#17606=AXIS2_PLACEMENT_3D('',#36234,#21336,#21337);
#17607=AXIS2_PLACEMENT_3D('',#36235,#21338,#21339);
#17608=AXIS2_PLACEMENT_3D('',#36236,#21340,#21341);
#17609=AXIS2_PLACEMENT_3D('',#36237,#21342,#21343);
#17610=AXIS2_PLACEMENT_3D('',#36238,#21344,#21345);
#17611=AXIS2_PLACEMENT_3D('',#36239,#21346,#21347);
#17612=AXIS2_PLACEMENT_3D('',#36240,#21348,#21349);
#17613=AXIS2_PLACEMENT_3D('',#36241,#21350,#21351);
#17614=AXIS2_PLACEMENT_3D('',#36242,#21352,#21353);
#17615=AXIS2_PLACEMENT_3D('',#36243,#21354,#21355);
#17616=AXIS2_PLACEMENT_3D('',#36244,#21356,#21357);
#17617=AXIS2_PLACEMENT_3D('',#36245,#21358,#21359);
#17618=AXIS2_PLACEMENT_3D('',#36247,#21360,#21361);
#17619=AXIS2_PLACEMENT_3D('',#36248,#21362,#21363);
#17620=AXIS2_PLACEMENT_3D('',#36250,#21365,#21366);
#17621=AXIS2_PLACEMENT_3D('',#36252,#21367,#21368);
#17622=AXIS2_PLACEMENT_3D('',#36254,#21370,#21371);
#17623=AXIS2_PLACEMENT_3D('',#36255,#21372,#21373);
#17624=AXIS2_PLACEMENT_3D('',#36256,#21374,#21375);
#17625=AXIS2_PLACEMENT_3D('',#36272,#21377,#21378);
#17626=AXIS2_PLACEMENT_3D('',#36280,#21379,#21380);
#17627=AXIS2_PLACEMENT_3D('',#36328,#21382,#21383);
#17628=AXIS2_PLACEMENT_3D('',#36376,#21385,#21386);
#17629=AXIS2_PLACEMENT_3D('',#36430,#21388,#21389);
#17630=AXIS2_PLACEMENT_3D('',#36478,#21391,#21392);
#17631=AXIS2_PLACEMENT_3D('',#36526,#21394,#21395);
#17632=AXIS2_PLACEMENT_3D('',#36580,#21397,#21398);
#17633=AXIS2_PLACEMENT_3D('',#36628,#21400,#21401);
#17634=AXIS2_PLACEMENT_3D('',#36676,#21403,#21404);
#17635=AXIS2_PLACEMENT_3D('',#36724,#21406,#21407);
#17636=AXIS2_PLACEMENT_3D('',#36778,#21409,#21410);
#17637=AXIS2_PLACEMENT_3D('',#36790,#21412,#21413);
#17638=AXIS2_PLACEMENT_3D('',#36796,#21414,#21415);
#17639=AXIS2_PLACEMENT_3D('',#36821,#21417,#21418);
#17640=AXIS2_PLACEMENT_3D('',#36846,#21420,#21421);
#17641=AXIS2_PLACEMENT_3D('',#36870,#21423,#21424);
#17642=AXIS2_PLACEMENT_3D('',#36894,#21426,#21427);
#17643=AXIS2_PLACEMENT_3D('',#36919,#21429,#21430);
#17644=AXIS2_PLACEMENT_3D('',#36944,#21432,#21433);
#17645=AXIS2_PLACEMENT_3D('',#36968,#21435,#21436);
#17646=AXIS2_PLACEMENT_3D('',#36993,#21438,#21439);
#17647=AXIS2_PLACEMENT_3D('',#37018,#21441,#21442);
#17648=AXIS2_PLACEMENT_3D('',#37479,#21444,#21445);
#17649=AXIS2_PLACEMENT_3D('',#37481,#21446,#21447);
#17650=AXIS2_PLACEMENT_3D('',#37482,#21448,#21449);
#17651=AXIS2_PLACEMENT_3D('',#37539,#21450,#21451);
#17652=AXIS2_PLACEMENT_3D('',#37540,#21452,#21453);
#17653=AXIS2_PLACEMENT_3D('',#37918,#21454,#21455);
#17654=AXIS2_PLACEMENT_3D('',#37931,#21458,#21459);
#17655=AXIS2_PLACEMENT_3D('',#37941,#21461,#21462);
#17656=AXIS2_PLACEMENT_3D('',#37954,#21465,#21466);
#17657=AXIS2_PLACEMENT_3D('',#37964,#21468,#21469);
#17658=AXIS2_PLACEMENT_3D('',#37977,#21472,#21473);
#17659=AXIS2_PLACEMENT_3D('',#37987,#21475,#21476);
#17660=AXIS2_PLACEMENT_3D('',#38000,#21479,#21480);
#17661=AXIS2_PLACEMENT_3D('',#38010,#21482,#21483);
#17662=AXIS2_PLACEMENT_3D('',#38023,#21486,#21487);
#17663=AXIS2_PLACEMENT_3D('',#38033,#21489,#21490);
#17664=AXIS2_PLACEMENT_3D('',#38046,#21493,#21494);
#17665=AXIS2_PLACEMENT_3D('',#38056,#21496,#21497);
#17666=AXIS2_PLACEMENT_3D('',#38069,#21500,#21501);
#17667=AXIS2_PLACEMENT_3D('',#38079,#21503,#21504);
#17668=AXIS2_PLACEMENT_3D('',#38092,#21507,#21508);
#17669=AXIS2_PLACEMENT_3D('',#38102,#21510,#21511);
#17670=AXIS2_PLACEMENT_3D('',#38115,#21514,#21515);
#17671=AXIS2_PLACEMENT_3D('',#38125,#21517,#21518);
#17672=AXIS2_PLACEMENT_3D('',#38138,#21521,#21522);
#17673=AXIS2_PLACEMENT_3D('',#38148,#21524,#21525);
#17674=AXIS2_PLACEMENT_3D('',#38161,#21528,#21529);
#17675=AXIS2_PLACEMENT_3D('',#38171,#21531,#21532);
#17676=AXIS2_PLACEMENT_3D('',#38184,#21535,#21536);
#17677=AXIS2_PLACEMENT_3D('',#38194,#21538,#21539);
#17678=AXIS2_PLACEMENT_3D('',#38207,#21542,#21543);
#17679=AXIS2_PLACEMENT_3D('',#38217,#21545,#21546);
#17680=AXIS2_PLACEMENT_3D('',#38230,#21549,#21550);
#17681=AXIS2_PLACEMENT_3D('',#38240,#21552,#21553);
#17682=AXIS2_PLACEMENT_3D('',#38253,#21556,#21557);
#17683=AXIS2_PLACEMENT_3D('',#38263,#21559,#21560);
#17684=AXIS2_PLACEMENT_3D('',#38276,#21563,#21564);
#17685=AXIS2_PLACEMENT_3D('',#38286,#21566,#21567);
#17686=AXIS2_PLACEMENT_3D('',#38299,#21570,#21571);
#17687=AXIS2_PLACEMENT_3D('',#38309,#21573,#21574);
#17688=AXIS2_PLACEMENT_3D('',#38322,#21577,#21578);
#17689=AXIS2_PLACEMENT_3D('',#38332,#21580,#21581);
#17690=AXIS2_PLACEMENT_3D('',#38345,#21584,#21585);
#17691=AXIS2_PLACEMENT_3D('',#38355,#21587,#21588);
#17692=AXIS2_PLACEMENT_3D('',#38368,#21591,#21592);
#17693=AXIS2_PLACEMENT_3D('',#38378,#21594,#21595);
#17694=AXIS2_PLACEMENT_3D('',#38391,#21598,#21599);
#17695=AXIS2_PLACEMENT_3D('',#38401,#21601,#21602);
#17696=AXIS2_PLACEMENT_3D('',#38414,#21605,#21606);
#17697=AXIS2_PLACEMENT_3D('',#38424,#21608,#21609);
#17698=AXIS2_PLACEMENT_3D('',#38437,#21612,#21613);
#17699=AXIS2_PLACEMENT_3D('',#38447,#21615,#21616);
#17700=AXIS2_PLACEMENT_3D('',#38460,#21619,#21620);
#17701=AXIS2_PLACEMENT_3D('',#38470,#21622,#21623);
#17702=AXIS2_PLACEMENT_3D('',#38471,#21624,#21625);
#17703=AXIS2_PLACEMENT_3D('',#38472,#21626,#21627);
#17704=AXIS2_PLACEMENT_3D('',#38473,#21628,#21629);
#17705=AXIS2_PLACEMENT_3D('',#38474,#21630,#21631);
#17706=AXIS2_PLACEMENT_3D('',#38475,#21632,#21633);
#17707=AXIS2_PLACEMENT_3D('',#38476,#21634,#21635);
#17708=AXIS2_PLACEMENT_3D('',#38477,#21636,#21637);
#17709=AXIS2_PLACEMENT_3D('',#38478,#21638,#21639);
#17710=AXIS2_PLACEMENT_3D('',#38479,#21640,#21641);
#17711=AXIS2_PLACEMENT_3D('',#38480,#21642,#21643);
#17712=AXIS2_PLACEMENT_3D('',#38481,#21644,#21645);
#17713=AXIS2_PLACEMENT_3D('',#38482,#21646,#21647);
#17714=AXIS2_PLACEMENT_3D('',#38483,#21648,#21649);
#17715=AXIS2_PLACEMENT_3D('',#38484,#21650,#21651);
#17716=AXIS2_PLACEMENT_3D('',#38485,#21652,#21653);
#17717=AXIS2_PLACEMENT_3D('',#38486,#21654,#21655);
#17718=AXIS2_PLACEMENT_3D('',#38487,#21656,#21657);
#17719=AXIS2_PLACEMENT_3D('',#38488,#21658,#21659);
#17720=AXIS2_PLACEMENT_3D('',#38489,#21660,#21661);
#17721=AXIS2_PLACEMENT_3D('',#38490,#21662,#21663);
#17722=AXIS2_PLACEMENT_3D('',#38491,#21664,#21665);
#17723=AXIS2_PLACEMENT_3D('',#38492,#21666,#21667);
#17724=AXIS2_PLACEMENT_3D('',#38493,#21668,#21669);
#17725=AXIS2_PLACEMENT_3D('',#38494,#21670,#21671);
#17726=AXIS2_PLACEMENT_3D('',#38495,#21672,#21673);
#17727=AXIS2_PLACEMENT_3D('',#38496,#21674,#21675);
#17728=AXIS2_PLACEMENT_3D('',#38497,#21676,#21677);
#17729=AXIS2_PLACEMENT_3D('',#38498,#21678,#21679);
#17730=AXIS2_PLACEMENT_3D('',#38499,#21680,#21681);
#17731=AXIS2_PLACEMENT_3D('',#38500,#21682,#21683);
#17732=AXIS2_PLACEMENT_3D('',#38501,#21684,#21685);
#17733=AXIS2_PLACEMENT_3D('',#38502,#21686,#21687);
#17734=AXIS2_PLACEMENT_3D('',#38503,#21688,#21689);
#17735=AXIS2_PLACEMENT_3D('',#38504,#21690,#21691);
#17736=AXIS2_PLACEMENT_3D('',#38505,#21692,#21693);
#17737=AXIS2_PLACEMENT_3D('',#38506,#21694,#21695);
#17738=AXIS2_PLACEMENT_3D('',#38507,#21696,#21697);
#17739=AXIS2_PLACEMENT_3D('',#38508,#21698,#21699);
#17740=AXIS2_PLACEMENT_3D('',#38509,#21700,#21701);
#17741=AXIS2_PLACEMENT_3D('',#38510,#21702,#21703);
#17742=AXIS2_PLACEMENT_3D('',#38511,#21704,#21705);
#17743=AXIS2_PLACEMENT_3D('',#38512,#21706,#21707);
#17744=AXIS2_PLACEMENT_3D('',#38513,#21708,#21709);
#17745=AXIS2_PLACEMENT_3D('',#38514,#21710,#21711);
#17746=AXIS2_PLACEMENT_3D('',#38515,#21712,#21713);
#17747=AXIS2_PLACEMENT_3D('',#38516,#21714,#21715);
#17748=AXIS2_PLACEMENT_3D('',#38517,#21716,#21717);
#17749=AXIS2_PLACEMENT_3D('',#38518,#21718,#21719);
#17750=AXIS2_PLACEMENT_3D('',#38519,#21720,#21721);
#17751=AXIS2_PLACEMENT_3D('',#38520,#21722,#21723);
#17752=AXIS2_PLACEMENT_3D('',#38521,#21724,#21725);
#17753=AXIS2_PLACEMENT_3D('',#38522,#21726,#21727);
#17754=AXIS2_PLACEMENT_3D('',#38523,#21728,#21729);
#17755=AXIS2_PLACEMENT_3D('',#38524,#21730,#21731);
#17756=AXIS2_PLACEMENT_3D('',#38525,#21732,#21733);
#17757=AXIS2_PLACEMENT_3D('',#38526,#21734,#21735);
#17758=AXIS2_PLACEMENT_3D('',#38527,#21736,#21737);
#17759=AXIS2_PLACEMENT_3D('',#38528,#21738,#21739);
#17760=AXIS2_PLACEMENT_3D('',#38529,#21740,#21741);
#17761=AXIS2_PLACEMENT_3D('',#38530,#21742,#21743);
#17762=AXIS2_PLACEMENT_3D('',#38531,#21744,#21745);
#17763=AXIS2_PLACEMENT_3D('',#38532,#21746,#21747);
#17764=AXIS2_PLACEMENT_3D('',#38533,#21748,#21749);
#17765=AXIS2_PLACEMENT_3D('',#38534,#21750,#21751);
#17766=AXIS2_PLACEMENT_3D('',#38535,#21752,#21753);
#17767=AXIS2_PLACEMENT_3D('',#38536,#21754,#21755);
#17768=AXIS2_PLACEMENT_3D('',#38537,#21756,#21757);
#17769=AXIS2_PLACEMENT_3D('',#38538,#21758,#21759);
#17770=AXIS2_PLACEMENT_3D('',#38539,#21760,#21761);
#17771=AXIS2_PLACEMENT_3D('',#38540,#21762,#21763);
#17772=AXIS2_PLACEMENT_3D('',#38541,#21764,#21765);
#17773=AXIS2_PLACEMENT_3D('',#38542,#21766,#21767);
#17774=AXIS2_PLACEMENT_3D('',#38545,#21769,#21770);
#17775=AXIS2_PLACEMENT_3D('',#38546,#21771,#21772);
#17776=AXIS2_PLACEMENT_3D('',#38548,#21773,#21774);
#17777=AXIS2_PLACEMENT_3D('',#38549,#21775,#21776);
#17778=AXIS2_PLACEMENT_3D('',#38551,#21778,#21779);
#17779=AXIS2_PLACEMENT_3D('',#38552,#21780,#21781);
#17780=AXIS2_PLACEMENT_3D('',#38553,#21782,#21783);
#17781=AXIS2_PLACEMENT_3D('',#38554,#21784,#21785);
#17782=AXIS2_PLACEMENT_3D('',#38556,#21786,#21787);
#17783=AXIS2_PLACEMENT_3D('',#38558,#21789,#21790);
#17784=AXIS2_PLACEMENT_3D('',#38559,#21791,#21792);
#17785=AXIS2_PLACEMENT_3D('',#38560,#21793,#21794);
#17786=AXIS2_PLACEMENT_3D('',#38561,#21795,#21796);
#17787=AXIS2_PLACEMENT_3D('',#38562,#21797,#21798);
#17788=AXIS2_PLACEMENT_3D('',#38563,#21799,#21800);
#17789=AXIS2_PLACEMENT_3D('',#38564,#21801,#21802);
#17790=AXIS2_PLACEMENT_3D('',#38565,#21803,#21804);
#17791=AXIS2_PLACEMENT_3D('',#38566,#21805,#21806);
#17792=AXIS2_PLACEMENT_3D('',#38567,#21807,#21808);
#17793=AXIS2_PLACEMENT_3D('',#38568,#21809,#21810);
#17794=AXIS2_PLACEMENT_3D('',#38569,#21811,#21812);
#17795=AXIS2_PLACEMENT_3D('',#38570,#21813,#21814);
#17796=AXIS2_PLACEMENT_3D('',#38571,#21815,#21816);
#17797=AXIS2_PLACEMENT_3D('',#38572,#21817,#21818);
#17798=AXIS2_PLACEMENT_3D('',#38573,#21819,#21820);
#17799=AXIS2_PLACEMENT_3D('',#38574,#21821,#21822);
#17800=AXIS2_PLACEMENT_3D('',#38575,#21823,#21824);
#17801=AXIS2_PLACEMENT_3D('',#38576,#21825,#21826);
#17802=AXIS2_PLACEMENT_3D('',#38577,#21827,#21828);
#17803=AXIS2_PLACEMENT_3D('',#38578,#21829,#21830);
#17804=AXIS2_PLACEMENT_3D('',#38579,#21831,#21832);
#17805=DIRECTION('axis',(0.,0.,1.));
#17806=DIRECTION('refdir',(1.,0.,0.));
#17807=DIRECTION('axis',(0.,0.,1.));
#17808=DIRECTION('refdir',(1.,0.,0.));
#17809=DIRECTION('center_axis',(0.707106781186553,-0.707106781186542,0.));
#17810=DIRECTION('ref_axis',(0.,0.,-1.));
#17811=DIRECTION('',(0.577350269189623,0.577350269189632,0.577350269189623));
#17812=DIRECTION('',(0.,0.,1.));
#17813=DIRECTION('',(-0.577350269189623,-0.577350269189632,0.577350269189623));
#17814=DIRECTION('',(-0.57735026918962,-0.577350269189629,-0.577350269189629));
#17815=DIRECTION('',(0.,0.,-1.));
#17816=DIRECTION('',(0.57735026918962,0.577350269189629,-0.577350269189629));
#17817=DIRECTION('center_axis',(0.,-0.707106781186548,0.707106781186548));
#17818=DIRECTION('ref_axis',(1.,0.,0.));
#17819=DIRECTION('',(0.577350269189629,-0.577350269189623,-0.577350269189625));
#17820=DIRECTION('',(1.,0.,0.));
#17821=DIRECTION('',(0.,0.707106781186548,0.707106781186548));
#17822=DIRECTION('',(1.,0.,0.));
#17823=DIRECTION('center_axis',(0.707106781186548,0.,0.707106781186548));
#17824=DIRECTION('ref_axis',(0.707106781186548,0.,-0.707106781186548));
#17825=DIRECTION('',(0.,1.,0.));
#17826=DIRECTION('',(0.577350269189619,-0.57735026918964,-0.577350269189619));
#17827=DIRECTION('',(0.577350269189627,0.577350269189623,-0.577350269189627));
#17828=DIRECTION('',(0.,1.,0.));
#17829=DIRECTION('center_axis',(1.,0.,0.));
#17830=DIRECTION('ref_axis',(0.,1.,0.));
#17831=DIRECTION('',(0.,-1.,0.));
#17832=DIRECTION('',(0.,0.,-1.));
#17833=DIRECTION('center_axis',(0.707106781186561,0.707106781186534,0.));
#17834=DIRECTION('ref_axis',(0.,0.,-1.));
#17835=DIRECTION('',(-0.577350269189619,0.57735026918964,-0.577350269189618));
#17836=DIRECTION('',(-0.577350269189612,0.577350269189633,0.577350269189633));
#17837=DIRECTION('',(0.,0.,1.));
#17838=DIRECTION('',(0.577350269189612,-0.577350269189633,0.577350269189633));
#17839=DIRECTION('center_axis',(0.,0.707106781186548,0.707106781186548));
#17840=DIRECTION('ref_axis',(1.,0.,0.));
#17841=DIRECTION('',(-1.,0.,0.));
#17842=DIRECTION('',(0.,-0.707106781186548,0.707106781186548));
#17843=DIRECTION('',(-1.,0.,0.));
#17844=DIRECTION('center_axis',(0.707106781186558,0.707106781186537,0.));
#17845=DIRECTION('ref_axis',(0.,0.,-1.));
#17846=DIRECTION('',(0.57735026918962,-0.577350269189637,-0.57735026918962));
#17847=DIRECTION('',(0.,0.,-1.));
#17848=DIRECTION('',(-0.57735026918962,0.577350269189637,-0.57735026918962));
#17849=DIRECTION('',(-0.577350269189614,0.577350269189632,0.577350269189632));
#17850=DIRECTION('',(0.,0.,1.));
#17851=DIRECTION('',(0.577350269189614,-0.577350269189632,0.577350269189632));
#17852=DIRECTION('center_axis',(1.,0.,0.));
#17853=DIRECTION('ref_axis',(0.,1.,0.));
#17854=DIRECTION('',(0.,1.,0.));
#17855=DIRECTION('',(0.,0.,1.));
#17856=DIRECTION('',(0.,-1.,0.));
#17857=DIRECTION('center_axis',(0.707106781186548,0.,0.707106781186548));
#17858=DIRECTION('ref_axis',(0.707106781186548,0.,-0.707106781186548));
#17859=DIRECTION('',(0.577350269189627,0.577350269189624,-0.577350269189627));
#17860=DIRECTION('',(0.,1.,0.));
#17861=DIRECTION('',(-0.70710678118655,0.,0.707106781186545));
#17862=DIRECTION('center_axis',(0.,0.707106781186548,0.707106781186548));
#17863=DIRECTION('ref_axis',(1.,0.,0.));
#17864=DIRECTION('',(-1.,0.,0.));
#17865=DIRECTION('',(0.,-0.707106781186548,0.707106781186548));
#17866=DIRECTION('',(-1.,0.,0.));
#17867=DIRECTION('center_axis',(-0.707106781186555,0.70710678118654,0.));
#17868=DIRECTION('ref_axis',(0.,0.,1.));
#17869=DIRECTION('',(-0.577350269189622,-0.577350269189635,0.577350269189621));
#17870=DIRECTION('',(0.,0.,1.));
#17871=DIRECTION('',(0.577350269189622,0.577350269189634,0.577350269189622));
#17872=DIRECTION('',(0.577350269189617,0.57735026918963,-0.57735026918963));
#17873=DIRECTION('',(0.,0.,-1.));
#17874=DIRECTION('',(-0.577350269189617,-0.57735026918963,-0.57735026918963));
#17875=DIRECTION('center_axis',(-0.707106781186548,0.,0.707106781186548));
#17876=DIRECTION('ref_axis',(0.707106781186548,0.,0.707106781186548));
#17877=DIRECTION('',(0.,-1.,0.));
#17878=DIRECTION('',(0.707106781186548,0.,0.707106781186548));
#17879=DIRECTION('',(0.,-1.,0.));
#17880=DIRECTION('',(-0.577350269189629,0.577350269189623,-0.577350269189625));
#17881=DIRECTION('center_axis',(-1.,0.,0.));
#17882=DIRECTION('ref_axis',(0.,-1.,0.));
#17883=DIRECTION('',(0.,1.,0.));
#17884=DIRECTION('',(0.,0.,-1.));
#17885=DIRECTION('center_axis',(-0.707106781186547,0.,-0.707106781186548));
#17886=DIRECTION('ref_axis',(-0.707106781186548,0.,0.707106781186547));
#17887=DIRECTION('',(0.577350269189627,-0.577350269189624,-0.577350269189627));
#17888=DIRECTION('',(0.,-1.,0.));
#17889=DIRECTION('',(-0.707106781186548,0.,0.707106781186547));
#17890=DIRECTION('center_axis',(-0.707106781186561,-0.707106781186534,0.));
#17891=DIRECTION('ref_axis',(0.,0.,1.));
#17892=DIRECTION('',(-0.577350269189619,0.57735026918964,-0.577350269189619));
#17893=DIRECTION('',(0.,0.,-1.));
#17894=DIRECTION('',(0.577350269189619,-0.57735026918964,-0.577350269189618));
#17895=DIRECTION('',(0.577350269189612,-0.577350269189633,0.577350269189633));
#17896=DIRECTION('',(0.,0.,1.));
#17897=DIRECTION('',(-0.577350269189612,0.577350269189633,0.577350269189633));
#17898=DIRECTION('center_axis',(-0.707106781186547,0.,-0.707106781186548));
#17899=DIRECTION('ref_axis',(-0.707106781186548,0.,0.707106781186547));
#17900=DIRECTION('',(0.,1.,0.));
#17901=DIRECTION('',(-0.577350269189623,-0.577350269189632,0.577350269189623));
#17902=DIRECTION('',(0.577350269189627,-0.577350269189624,-0.577350269189627));
#17903=DIRECTION('',(0.,-1.,0.));
#17904=DIRECTION('',(-0.577350269189627,-0.577350269189624,0.577350269189627));
#17905=DIRECTION('center_axis',(-1.,0.,0.));
#17906=DIRECTION('ref_axis',(0.,-1.,0.));
#17907=DIRECTION('',(0.,-1.,0.));
#17908=DIRECTION('',(0.,0.,1.));
#17909=DIRECTION('center_axis',(-0.707106781186548,0.,0.707106781186548));
#17910=DIRECTION('ref_axis',(0.707106781186548,0.,0.707106781186548));
#17911=DIRECTION('',(-0.577350269189627,-0.577350269189623,-0.577350269189627));
#17912=DIRECTION('',(0.,-1.,0.));
#17913=DIRECTION('',(-0.577350269189629,0.577350269189623,-0.577350269189625));
#17914=DIRECTION('',(0.577350269189623,0.577350269189632,0.577350269189623));
#17915=DIRECTION('center_axis',(-0.707106781186553,0.707106781186542,0.));
#17916=DIRECTION('ref_axis',(0.,0.,1.));
#17917=DIRECTION('',(0.57735026918962,0.577350269189629,-0.577350269189629));
#17918=DIRECTION('',(0.,0.,-1.));
#17919=DIRECTION('',(-0.57735026918962,-0.577350269189629,-0.577350269189629));
#17920=DIRECTION('center_axis',(0.,2.96961385686688E-15,1.));
#17921=DIRECTION('ref_axis',(1.,2.98726371833858E-17,0.));
#17922=DIRECTION('center_axis',(0.,0.,-1.));
#17923=DIRECTION('ref_axis',(1.,6.12323399573676E-17,0.));
#17924=DIRECTION('',(-0.923879532511288,1.22196591669764E-15,0.382683432365087));
#17925=DIRECTION('center_axis',(0.,0.,1.));
#17926=DIRECTION('ref_axis',(1.,0.,0.));
#17927=DIRECTION('center_axis',(0.,0.,1.));
#17928=DIRECTION('ref_axis',(1.,0.,0.));
#17929=DIRECTION('',(0.707106781186547,8.65956056235493E-17,-0.707106781186547));
#17930=DIRECTION('center_axis',(0.,0.,1.));
#17931=DIRECTION('ref_axis',(1.,6.12323399573677E-17,0.));
#17932=DIRECTION('center_axis',(0.,0.,1.));
#17933=DIRECTION('ref_axis',(1.,0.,0.));
#17934=DIRECTION('center_axis',(0.,0.,-1.));
#17935=DIRECTION('ref_axis',(1.,0.,0.));
#17936=DIRECTION('center_axis',(0.,-1.22099907537238E-15,1.));
#17937=DIRECTION('ref_axis',(1.,3.09374953297515E-17,0.));
#17938=DIRECTION('',(0.382683432365087,1.18676052590658E-15,-0.923879532511288));
#17939=DIRECTION('center_axis',(0.,0.,-1.));
#17940=DIRECTION('ref_axis',(1.,0.,0.));
#17941=DIRECTION('center_axis',(0.,0.,-1.));
#17942=DIRECTION('ref_axis',(1.,0.,0.));
#17943=DIRECTION('',(0.,0.,-1.));
#17944=DIRECTION('center_axis',(0.,0.,-1.));
#17945=DIRECTION('ref_axis',(1.,0.,0.));
#17946=DIRECTION('',(-0.62463654800244,0.780915605491141,4.73897997350133E-15));
#17947=DIRECTION('center_axis',(0.,1.,0.));
#17948=DIRECTION('ref_axis',(0.,0.,1.));
#17949=DIRECTION('',(0.,1.,0.));
#17950=DIRECTION('center_axis',(0.707106781186555,-0.70710678118654,0.));
#17951=DIRECTION('ref_axis',(0.,0.,-1.));
#17952=DIRECTION('',(0.577350269189622,0.577350269189635,0.577350269189621));
#17953=DIRECTION('',(0.,0.,1.));
#17954=DIRECTION('',(-0.357406744336599,-0.357406744336607,0.862856209461009));
#17955=DIRECTION('',(-0.577350269189617,-0.57735026918963,-0.57735026918963));
#17956=DIRECTION('',(0.,0.,-1.));
#17957=DIRECTION('',(0.577350269189617,0.57735026918963,-0.57735026918963));
#17958=DIRECTION('center_axis',(0.,1.,0.));
#17959=DIRECTION('ref_axis',(1.,0.,0.));
#17960=DIRECTION('',(1.,0.,0.));
#17961=DIRECTION('',(0.,0.,-1.));
#17962=DIRECTION('',(-1.,0.,0.));
#17963=DIRECTION('center_axis',(0.,-0.707106781186548,0.707106781186548));
#17964=DIRECTION('ref_axis',(1.,0.,0.));
#17965=DIRECTION('',(0.281084637714827,-0.678598344545846,-0.678598344545846));
#17966=DIRECTION('',(0.577350269189629,-0.577350269189623,-0.577350269189625));
#17967=DIRECTION('',(1.,0.,0.));
#17968=DIRECTION('',(0.,0.707106781186548,0.707106781186548));
#17969=DIRECTION('center_axis',(0.923879532511283,0.,0.382683432365098));
#17970=DIRECTION('ref_axis',(0.382683432365098,0.,-0.923879532511283));
#17971=DIRECTION('',(0.,1.,0.));
#17972=DIRECTION('',(-0.38268343236509,0.,0.923879532511287));
#17973=DIRECTION('',(0.,-1.,0.));
#17974=DIRECTION('center_axis',(-0.707106781186558,-0.707106781186537,0.));
#17975=DIRECTION('ref_axis',(0.,0.,1.));
#17976=DIRECTION('',(-0.357406744336599,0.357406744336609,-0.862856209461008));
#17977=DIRECTION('',(0.,0.,-1.));
#17978=DIRECTION('',(0.57735026918962,-0.577350269189637,-0.57735026918962));
#17979=DIRECTION('',(0.577350269189614,-0.577350269189632,0.577350269189632));
#17980=DIRECTION('',(0.,0.,1.));
#17981=DIRECTION('',(-0.577350269189614,0.577350269189632,0.577350269189632));
#17982=DIRECTION('center_axis',(-0.707106781186547,0.,-0.707106781186548));
#17983=DIRECTION('ref_axis',(-0.707106781186548,0.,0.707106781186547));
#17984=DIRECTION('',(0.,1.,0.));
#17985=DIRECTION('',(-0.707106781186556,0.,0.707106781186539));
#17986=DIRECTION('',(0.,-1.,0.));
#17987=DIRECTION('',(-0.577350269189627,-0.577350269189624,0.577350269189627));
#17988=DIRECTION('center_axis',(-1.,0.,0.));
#17989=DIRECTION('ref_axis',(0.,-1.,0.));
#17990=DIRECTION('',(0.,-1.,0.));
#17991=DIRECTION('',(0.,0.,1.));
#17992=DIRECTION('center_axis',(-0.923879532511283,0.,0.382683432365098));
#17993=DIRECTION('ref_axis',(0.382683432365098,0.,0.923879532511283));
#17994=DIRECTION('',(0.281084637714827,0.678598344545846,0.678598344545846));
#17995=DIRECTION('',(0.,1.,0.));
#17996=DIRECTION('',(0.382683432365096,0.,0.923879532511284));
#17997=DIRECTION('center_axis',(0.,0.,-1.));
#17998=DIRECTION('ref_axis',(0.707106781186548,0.707106781186548,0.));
#17999=DIRECTION('',(0.,-0.382683432365096,0.923879532511284));
#18000=DIRECTION('center_axis',(0.,0.,-1.));
#18001=DIRECTION('ref_axis',(0.707106781186548,0.707106781186548,0.));
#18002=DIRECTION('center_axis',(0.,0.,1.));
#18003=DIRECTION('ref_axis',(0.707106781186548,0.707106781186548,0.));
#18004=DIRECTION('center_axis',(0.,0.923879532511283,0.382683432365098));
#18005=DIRECTION('ref_axis',(0.,-0.382683432365098,0.923879532511283));
#18006=DIRECTION('',(0.,-0.38268343236509,0.923879532511287));
#18007=DIRECTION('',(1.,0.,0.));
#18008=DIRECTION('',(-1.,0.,0.));
#18009=DIRECTION('center_axis',(0.,0.,-1.));
#18010=DIRECTION('ref_axis',(-0.707106781186548,0.707106781186548,0.));
#18011=DIRECTION('center_axis',(0.,0.,-1.));
#18012=DIRECTION('ref_axis',(-0.707106781186548,0.707106781186548,0.));
#18013=DIRECTION('center_axis',(0.,0.,1.));
#18014=DIRECTION('ref_axis',(-0.707106781186548,0.707106781186548,0.));
#18015=DIRECTION('center_axis',(0.,-0.707106781186548,0.707106781186548));
#18016=DIRECTION('ref_axis',(1.,0.,0.));
#18017=DIRECTION('',(1.,0.,0.));
#18018=DIRECTION('',(0.,0.707106781186548,0.707106781186548));
#18019=DIRECTION('',(1.,0.,0.));
#18020=DIRECTION('',(-0.577350269189627,-0.577350269189624,-0.577350269189627));
#18021=DIRECTION('center_axis',(0.,1.,0.));
#18022=DIRECTION('ref_axis',(1.,0.,0.));
#18023=DIRECTION('',(-1.,0.,0.));
#18024=DIRECTION('',(0.,0.,-1.));
#18025=DIRECTION('center_axis',(0.,0.,1.));
#18026=DIRECTION('ref_axis',(-0.707106781186547,0.707106781186547,0.));
#18027=DIRECTION('',(0.,0.,-1.));
#18028=DIRECTION('center_axis',(0.,0.,-1.));
#18029=DIRECTION('ref_axis',(-0.707106781186548,0.707106781186548,0.));
#18030=DIRECTION('center_axis',(0.,1.,0.));
#18031=DIRECTION('ref_axis',(-1.,0.,0.));
#18032=DIRECTION('',(0.,0.,1.));
#18033=DIRECTION('',(1.,0.,0.));
#18034=DIRECTION('center_axis',(0.,0.,1.));
#18035=DIRECTION('ref_axis',(0.707106781186547,0.707106781186547,0.));
#18036=DIRECTION('',(0.,0.,-1.));
#18037=DIRECTION('center_axis',(0.,0.,-1.));
#18038=DIRECTION('ref_axis',(0.707106781186548,0.707106781186548,0.));
#18039=DIRECTION('center_axis',(1.,0.,0.));
#18040=DIRECTION('ref_axis',(0.,1.,0.));
#18041=DIRECTION('',(0.,-1.,0.));
#18042=DIRECTION('center_axis',(-0.382683432365098,0.,0.923879532511283));
#18043=DIRECTION('ref_axis',(0.923879532511283,0.,0.382683432365098));
#18044=DIRECTION('',(0.678598344545834,0.678598344545859,0.281084637714822));
#18045=DIRECTION('',(0.,1.,0.));
#18046=DIRECTION('',(-0.923879532511283,0.,-0.382683432365098));
#18047=DIRECTION('',(0.,-1.,0.));
#18048=DIRECTION('center_axis',(0.,0.,-1.));
#18049=DIRECTION('ref_axis',(-0.707106781186548,0.707106781186548,0.));
#18050=DIRECTION('',(0.,0.923879532511291,-0.38268343236508));
#18051=DIRECTION('center_axis',(0.,0.,1.));
#18052=DIRECTION('ref_axis',(-0.707106781186548,0.707106781186548,0.));
#18053=DIRECTION('center_axis',(0.,0.,-1.));
#18054=DIRECTION('ref_axis',(-0.707106781186548,0.707106781186548,0.));
#18055=DIRECTION('center_axis',(0.,0.382683432365103,0.923879532511281));
#18056=DIRECTION('ref_axis',(1.,0.,0.));
#18057=DIRECTION('',(0.,0.923879532511281,-0.382683432365103));
#18058=DIRECTION('',(-1.,0.,0.));
#18059=DIRECTION('',(1.,0.,0.));
#18060=DIRECTION('center_axis',(0.,0.,-1.));
#18061=DIRECTION('ref_axis',(0.707106781186548,0.707106781186548,0.));
#18062=DIRECTION('',(0.923879532511291,0.,-0.38268343236508));
#18063=DIRECTION('center_axis',(0.,0.,1.));
#18064=DIRECTION('ref_axis',(0.707106781186548,0.707106781186548,0.));
#18065=DIRECTION('center_axis',(0.,0.,-1.));
#18066=DIRECTION('ref_axis',(0.707106781186548,0.707106781186548,0.));
#18067=DIRECTION('center_axis',(0.382683432365098,0.,0.923879532511283));
#18068=DIRECTION('ref_axis',(0.923879532511283,0.,-0.382683432365098));
#18069=DIRECTION('',(0.678598344545834,-0.678598344545859,-0.281084637714822));
#18070=DIRECTION('',(0.,1.,0.));
#18071=DIRECTION('',(0.,-1.,0.));
#18072=DIRECTION('center_axis',(-0.707106781186548,0.,0.707106781186548));
#18073=DIRECTION('ref_axis',(0.707106781186548,0.,0.707106781186548));
#18074=DIRECTION('',(0.70710678118655,0.,0.707106781186545));
#18075=DIRECTION('center_axis',(0.,0.,-1.));
#18076=DIRECTION('ref_axis',(-0.707106781186547,0.707106781186547,0.));
#18077=DIRECTION('',(0.,-0.707106781186548,0.707106781186548));
#18078=DIRECTION('center_axis',(0.,0.707106781186548,0.707106781186548));
#18079=DIRECTION('ref_axis',(1.,0.,0.));
#18080=DIRECTION('',(0.,-0.70710678118655,0.707106781186545));
#18081=DIRECTION('center_axis',(0.,0.,-1.));
#18082=DIRECTION('ref_axis',(0.707106781186547,0.707106781186547,0.));
#18083=DIRECTION('',(-0.707106781186548,0.,0.707106781186548));
#18084=DIRECTION('center_axis',(0.707106781186548,0.,0.707106781186548));
#18085=DIRECTION('ref_axis',(0.707106781186548,0.,-0.707106781186548));
#18086=DIRECTION('center_axis',(0.,-0.382683432365086,0.923879532511289));
#18087=DIRECTION('ref_axis',(1.,0.,0.));
#18088=DIRECTION('',(-1.,0.,0.));
#18089=DIRECTION('',(0.,-0.923879532511289,-0.382683432365086));
#18090=DIRECTION('center_axis',(0.,0.,1.));
#18091=DIRECTION('ref_axis',(0.,1.,0.));
#18092=DIRECTION('',(0.,0.923879532511287,-0.38268343236509));
#18093=DIRECTION('center_axis',(0.,0.,-1.));
#18094=DIRECTION('ref_axis',(0.,1.,0.));
#18095=DIRECTION('center_axis',(0.,0.,1.));
#18096=DIRECTION('ref_axis',(0.,1.,0.));
#18097=DIRECTION('center_axis',(0.,0.382683432365089,0.923879532511287));
#18098=DIRECTION('ref_axis',(1.,0.,0.));
#18099=DIRECTION('',(1.,0.,0.));
#18100=DIRECTION('',(0.678598344545841,0.678598344545853,-0.281084637714822));
#18101=DIRECTION('center_axis',(0.382683432365098,0.,0.923879532511283));
#18102=DIRECTION('ref_axis',(0.923879532511283,0.,-0.382683432365098));
#18103=DIRECTION('',(0.,-1.,0.));
#18104=DIRECTION('',(0.678598344545841,-0.678598344545852,-0.281084637714823));
#18105=DIRECTION('center_axis',(0.,-0.382683432365089,0.923879532511287));
#18106=DIRECTION('ref_axis',(1.,0.,0.));
#18107=DIRECTION('',(-1.,0.,0.));
#18108=DIRECTION('',(0.,-0.923879532511287,-0.38268343236509));
#18109=DIRECTION('center_axis',(0.,0.,1.));
#18110=DIRECTION('ref_axis',(0.,1.,0.));
#18111=DIRECTION('',(0.,0.923879532511287,-0.38268343236509));
#18112=DIRECTION('center_axis',(0.,0.,-1.));
#18113=DIRECTION('ref_axis',(0.,1.,0.));
#18114=DIRECTION('center_axis',(0.,0.,1.));
#18115=DIRECTION('ref_axis',(0.,1.,0.));
#18116=DIRECTION('center_axis',(0.,0.382683432365086,0.923879532511289));
#18117=DIRECTION('ref_axis',(1.,0.,0.));
#18118=DIRECTION('',(1.,0.,0.));
#18119=DIRECTION('',(0.67859834454584,0.678598344545855,-0.28108463771482));
#18120=DIRECTION('center_axis',(0.382683432365098,0.,0.923879532511283));
#18121=DIRECTION('ref_axis',(0.923879532511283,0.,-0.382683432365098));
#18122=DIRECTION('',(0.,-1.,0.));
#18123=DIRECTION('',(0.923879532511283,0.,-0.382683432365098));
#18124=DIRECTION('center_axis',(0.,0.,-1.));
#18125=DIRECTION('ref_axis',(0.707106781186548,-0.707106781186548,0.));
#18126=DIRECTION('',(0.,-0.923879532511291,-0.38268343236508));
#18127=DIRECTION('center_axis',(0.,0.,1.));
#18128=DIRECTION('ref_axis',(0.707106781186548,-0.707106781186548,0.));
#18129=DIRECTION('center_axis',(0.,0.,-1.));
#18130=DIRECTION('ref_axis',(0.707106781186548,-0.707106781186548,0.));
#18131=DIRECTION('center_axis',(0.,-0.382683432365103,0.923879532511281));
#18132=DIRECTION('ref_axis',(1.,0.,0.));
#18133=DIRECTION('',(0.,-0.923879532511281,-0.382683432365103));
#18134=DIRECTION('',(1.,0.,0.));
#18135=DIRECTION('',(-1.,0.,0.));
#18136=DIRECTION('center_axis',(0.,0.,-1.));
#18137=DIRECTION('ref_axis',(-0.707106781186548,-0.707106781186548,0.));
#18138=DIRECTION('',(-0.923879532511291,0.,-0.38268343236508));
#18139=DIRECTION('center_axis',(0.,0.,1.));
#18140=DIRECTION('ref_axis',(-0.707106781186548,-0.707106781186548,0.));
#18141=DIRECTION('center_axis',(0.,0.,-1.));
#18142=DIRECTION('ref_axis',(-0.707106781186548,-0.707106781186548,0.));
#18143=DIRECTION('center_axis',(-0.382683432365098,0.,0.923879532511283));
#18144=DIRECTION('ref_axis',(0.923879532511283,0.,0.382683432365098));
#18145=DIRECTION('',(0.,1.,0.));
#18146=DIRECTION('',(-0.678598344545837,0.678598344545857,-0.281084637714821));
#18147=DIRECTION('center_axis',(0.,0.382683432365086,0.923879532511289));
#18148=DIRECTION('ref_axis',(1.,0.,0.));
#18149=DIRECTION('',(1.,0.,0.));
#18150=DIRECTION('',(0.,0.923879532511289,-0.382683432365086));
#18151=DIRECTION('',(-1.,0.,0.));
#18152=DIRECTION('center_axis',(0.,0.,1.));
#18153=DIRECTION('ref_axis',(0.,-1.,0.));
#18154=DIRECTION('',(0.,-0.923879532511287,-0.38268343236509));
#18155=DIRECTION('center_axis',(0.,0.,-1.));
#18156=DIRECTION('ref_axis',(0.,-1.,0.));
#18157=DIRECTION('center_axis',(0.,0.,1.));
#18158=DIRECTION('ref_axis',(0.,-1.,0.));
#18159=DIRECTION('center_axis',(0.,-0.382683432365089,0.923879532511287));
#18160=DIRECTION('ref_axis',(1.,0.,0.));
#18161=DIRECTION('',(1.,0.,0.));
#18162=DIRECTION('',(-1.,0.,0.));
#18163=DIRECTION('',(-0.678598344545841,-0.678598344545853,-0.281084637714822));
#18164=DIRECTION('center_axis',(-0.382683432365098,0.,0.923879532511283));
#18165=DIRECTION('ref_axis',(0.923879532511283,0.,0.382683432365098));
#18166=DIRECTION('',(0.,1.,0.));
#18167=DIRECTION('',(-0.678598344545841,0.678598344545852,-0.281084637714823));
#18168=DIRECTION('center_axis',(0.,0.382683432365089,0.923879532511287));
#18169=DIRECTION('ref_axis',(1.,0.,0.));
#18170=DIRECTION('',(1.,0.,0.));
#18171=DIRECTION('',(0.,0.923879532511287,-0.38268343236509));
#18172=DIRECTION('',(-1.,0.,0.));
#18173=DIRECTION('center_axis',(0.,0.,1.));
#18174=DIRECTION('ref_axis',(0.,-1.,0.));
#18175=DIRECTION('',(0.,-0.923879532511287,-0.38268343236509));
#18176=DIRECTION('center_axis',(0.,0.,-1.));
#18177=DIRECTION('ref_axis',(0.,-1.,0.));
#18178=DIRECTION('center_axis',(0.,0.,1.));
#18179=DIRECTION('ref_axis',(0.,-1.,0.));
#18180=DIRECTION('center_axis',(0.,-0.382683432365086,0.923879532511289));
#18181=DIRECTION('ref_axis',(1.,0.,0.));
#18182=DIRECTION('',(-1.,0.,0.));
#18183=DIRECTION('center_axis',(0.,0.,1.));
#18184=DIRECTION('ref_axis',(1.,0.,0.));
#18185=DIRECTION('center_axis',(0.,0.,1.));
#18186=DIRECTION('ref_axis',(1.,0.,0.));
#18187=DIRECTION('',(0.754127675160995,-0.656727835222685,5.63512495882306E-15));
#18188=DIRECTION('center_axis',(0.,0.,1.));
#18189=DIRECTION('ref_axis',(1.,0.,0.));
#18190=DIRECTION('center_axis',(0.,0.,1.));
#18191=DIRECTION('ref_axis',(1.,0.,0.));
#18192=DIRECTION('',(0.,0.,-1.));
#18193=DIRECTION('center_axis',(0.,0.,-1.));
#18194=DIRECTION('ref_axis',(1.,0.,0.));
#18195=DIRECTION('center_axis',(0.,0.,-1.));
#18196=DIRECTION('ref_axis',(1.,0.,0.));
#18197=DIRECTION('center_axis',(0.,1.88765402986373E-15,-1.));
#18198=DIRECTION('ref_axis',(1.,3.04118571122536E-17,0.));
#18199=DIRECTION('center_axis',(0.,0.,-1.));
#18200=DIRECTION('ref_axis',(1.,6.12323399573677E-17,0.));
#18201=DIRECTION('',(-0.38268343236509,1.68546160473598E-15,-0.923879532511286));
#18202=DIRECTION('center_axis',(0.,0.,-1.));
#18203=DIRECTION('ref_axis',(1.,0.,0.));
#18204=DIRECTION('',(-0.707106781186548,-8.65956056235493E-17,-0.707106781186548));
#18205=DIRECTION('center_axis',(0.,0.,-1.));
#18206=DIRECTION('ref_axis',(-1.,0.,0.));
#18207=DIRECTION('center_axis',(-1.22464679914735E-16,-1.,0.));
#18208=DIRECTION('ref_axis',(1.,-1.22464679914735E-16,0.));
#18209=DIRECTION('center_axis',(0.,0.,1.));
#18210=DIRECTION('ref_axis',(1.,0.,0.));
#18211=DIRECTION('center_axis',(0.707106781186547,0.,-0.707106781186548));
#18212=DIRECTION('ref_axis',(-0.707106781186548,0.,-0.707106781186547));
#18213=DIRECTION('',(-0.577350269189627,0.577350269189624,-0.577350269189627));
#18214=DIRECTION('',(0.,1.,0.));
#18215=DIRECTION('',(0.707106781186548,0.,0.707106781186547));
#18216=DIRECTION('center_axis',(0.707106781186547,0.,-0.707106781186548));
#18217=DIRECTION('ref_axis',(-0.707106781186548,0.,-0.707106781186547));
#18218=DIRECTION('',(-0.577350269189627,0.577350269189624,-0.577350269189627));
#18219=DIRECTION('',(0.,1.,0.));
#18220=DIRECTION('',(0.577350269189627,0.577350269189624,0.577350269189627));
#18221=DIRECTION('center_axis',(0.,0.,1.));
#18222=DIRECTION('ref_axis',(-0.707106781186547,-0.707106781186547,0.));
#18223=DIRECTION('',(0.,-0.707106781186556,0.707106781186539));
#18224=DIRECTION('center_axis',(0.,0.,-1.));
#18225=DIRECTION('ref_axis',(-0.707106781186548,-0.707106781186548,0.));
#18226=DIRECTION('center_axis',(0.,0.,1.));
#18227=DIRECTION('ref_axis',(-0.707106781186548,-0.707106781186548,0.));
#18228=DIRECTION('center_axis',(0.,-0.707106781186547,-0.707106781186548));
#18229=DIRECTION('ref_axis',(-1.,0.,0.));
#18230=DIRECTION('',(0.,-0.707106781186548,0.707106781186547));
#18231=DIRECTION('',(-1.,0.,0.));
#18232=DIRECTION('',(1.,0.,0.));
#18233=DIRECTION('center_axis',(0.,0.,1.));
#18234=DIRECTION('ref_axis',(0.707106781186547,-0.707106781186547,0.));
#18235=DIRECTION('',(0.707106781186556,0.,0.707106781186539));
#18236=DIRECTION('center_axis',(0.,0.,-1.));
#18237=DIRECTION('ref_axis',(0.707106781186548,-0.707106781186548,0.));
#18238=DIRECTION('center_axis',(0.,0.,1.));
#18239=DIRECTION('ref_axis',(0.707106781186548,-0.707106781186548,0.));
#18240=DIRECTION('center_axis',(0.707106781186547,0.,-0.707106781186548));
#18241=DIRECTION('ref_axis',(-0.707106781186548,0.,-0.707106781186547));
#18242=DIRECTION('',(0.,1.,0.));
#18243=DIRECTION('',(0.577350269189627,0.577350269189624,0.577350269189627));
#18244=DIRECTION('center_axis',(0.,0.707106781186548,-0.707106781186548));
#18245=DIRECTION('ref_axis',(-1.,0.,0.));
#18246=DIRECTION('',(1.,0.,0.));
#18247=DIRECTION('',(0.,-0.707106781186548,-0.707106781186548));
#18248=DIRECTION('',(-1.,0.,0.));
#18249=DIRECTION('center_axis',(0.,0.,-1.));
#18250=DIRECTION('ref_axis',(0.,-1.,0.));
#18251=DIRECTION('',(0.,0.707106781186548,-0.707106781186548));
#18252=DIRECTION('center_axis',(0.,0.,-1.));
#18253=DIRECTION('ref_axis',(0.,-1.,0.));
#18254=DIRECTION('center_axis',(0.,0.,1.));
#18255=DIRECTION('ref_axis',(0.,-1.,0.));
#18256=DIRECTION('center_axis',(0.,-0.707106781186548,-0.707106781186548));
#18257=DIRECTION('ref_axis',(-1.,0.,0.));
#18258=DIRECTION('',(1.,0.,0.));
#18259=DIRECTION('',(-1.,0.,0.));
#18260=DIRECTION('center_axis',(0.,-0.707106781186548,-0.707106781186548));
#18261=DIRECTION('ref_axis',(-1.,0.,0.));
#18262=DIRECTION('',(-1.,0.,0.));
#18263=DIRECTION('',(0.,0.707106781186548,-0.707106781186548));
#18264=DIRECTION('',(1.,0.,0.));
#18265=DIRECTION('center_axis',(0.,0.,-1.));
#18266=DIRECTION('ref_axis',(0.,1.,0.));
#18267=DIRECTION('',(0.,-0.707106781186548,-0.707106781186548));
#18268=DIRECTION('center_axis',(0.,0.,-1.));
#18269=DIRECTION('ref_axis',(0.,1.,0.));
#18270=DIRECTION('center_axis',(0.,0.,1.));
#18271=DIRECTION('ref_axis',(0.,1.,0.));
#18272=DIRECTION('center_axis',(0.,0.707106781186548,-0.707106781186548));
#18273=DIRECTION('ref_axis',(-1.,0.,0.));
#18274=DIRECTION('',(-1.,0.,0.));
#18275=DIRECTION('',(1.,0.,0.));
#18276=DIRECTION('center_axis',(0.,0.707106781186548,-0.707106781186548));
#18277=DIRECTION('ref_axis',(-1.,0.,0.));
#18278=DIRECTION('',(1.,0.,0.));
#18279=DIRECTION('',(0.,-0.707106781186548,-0.707106781186548));
#18280=DIRECTION('',(-1.,0.,0.));
#18281=DIRECTION('center_axis',(0.,0.,-1.));
#18282=DIRECTION('ref_axis',(0.,-1.,0.));
#18283=DIRECTION('',(0.,0.707106781186548,-0.707106781186548));
#18284=DIRECTION('center_axis',(0.,0.,-1.));
#18285=DIRECTION('ref_axis',(0.,-1.,0.));
#18286=DIRECTION('center_axis',(0.,0.,1.));
#18287=DIRECTION('ref_axis',(0.,-1.,0.));
#18288=DIRECTION('center_axis',(0.,-0.707106781186548,-0.707106781186548));
#18289=DIRECTION('ref_axis',(-1.,0.,0.));
#18290=DIRECTION('',(1.,0.,0.));
#18291=DIRECTION('center_axis',(0.,-0.707106781186548,-0.707106781186548));
#18292=DIRECTION('ref_axis',(-1.,0.,0.));
#18293=DIRECTION('',(0.,0.707106781186548,-0.707106781186548));
#18294=DIRECTION('',(1.,0.,0.));
#18295=DIRECTION('center_axis',(0.,0.,-1.));
#18296=DIRECTION('ref_axis',(0.,1.,0.));
#18297=DIRECTION('',(0.,-0.707106781186548,-0.707106781186548));
#18298=DIRECTION('center_axis',(0.,0.,-1.));
#18299=DIRECTION('ref_axis',(0.,1.,0.));
#18300=DIRECTION('center_axis',(0.,0.,1.));
#18301=DIRECTION('ref_axis',(0.,1.,0.));
#18302=DIRECTION('center_axis',(0.,0.707106781186548,-0.707106781186548));
#18303=DIRECTION('ref_axis',(-1.,0.,0.));
#18304=DIRECTION('',(-1.,0.,0.));
#18305=DIRECTION('',(1.,0.,0.));
#18306=DIRECTION('center_axis',(0.,0.,1.));
#18307=DIRECTION('ref_axis',(0.707106781186547,0.707106781186547,0.));
#18308=DIRECTION('',(0.,0.707106781186556,0.707106781186539));
#18309=DIRECTION('center_axis',(0.,0.,1.));
#18310=DIRECTION('ref_axis',(0.707106781186548,0.707106781186548,0.));
#18311=DIRECTION('center_axis',(0.,0.707106781186547,-0.707106781186548));
#18312=DIRECTION('ref_axis',(-1.,0.,0.));
#18313=DIRECTION('',(0.,0.707106781186548,0.707106781186547));
#18314=DIRECTION('',(-1.,0.,0.));
#18315=DIRECTION('center_axis',(0.,0.,1.));
#18316=DIRECTION('ref_axis',(-0.707106781186547,0.707106781186547,0.));
#18317=DIRECTION('center_axis',(0.,0.,1.));
#18318=DIRECTION('ref_axis',(-0.707106781186548,0.707106781186548,0.));
#18319=DIRECTION('center_axis',(0.,0.,-1.));
#18320=DIRECTION('ref_axis',(0.,-1.,0.));
#18321=DIRECTION('',(0.,0.,-1.));
#18322=DIRECTION('center_axis',(0.,0.,-1.));
#18323=DIRECTION('ref_axis',(0.,-1.,0.));
#18324=DIRECTION('center_axis',(0.,-1.,0.));
#18325=DIRECTION('ref_axis',(-1.,0.,0.));
#18326=DIRECTION('',(-1.,0.,0.));
#18327=DIRECTION('center_axis',(0.,1.,0.));
#18328=DIRECTION('ref_axis',(1.,0.,0.));
#18329=DIRECTION('',(0.,0.,-1.));
#18330=DIRECTION('',(1.,0.,0.));
#18331=DIRECTION('center_axis',(0.,0.,-1.));
#18332=DIRECTION('ref_axis',(0.,-1.,0.));
#18333=DIRECTION('',(0.,0.,-1.));
#18334=DIRECTION('center_axis',(0.,0.,-1.));
#18335=DIRECTION('ref_axis',(0.,-1.,0.));
#18336=DIRECTION('center_axis',(0.,-1.,0.));
#18337=DIRECTION('ref_axis',(-1.,0.,0.));
#18338=DIRECTION('',(-1.,0.,0.));
#18339=DIRECTION('center_axis',(0.,0.,1.));
#18340=DIRECTION('ref_axis',(1.,0.,0.));
#18341=DIRECTION('center_axis',(0.,0.,-1.));
#18342=DIRECTION('ref_axis',(-0.707106781186547,-0.707106781186547,0.));
#18343=DIRECTION('center_axis',(0.,0.,1.));
#18344=DIRECTION('ref_axis',(-0.707106781186548,-0.707106781186548,0.));
#18345=DIRECTION('',(0.,0.70710678118655,0.707106781186545));
#18346=DIRECTION('center_axis',(0.,-0.707106781186548,0.707106781186548));
#18347=DIRECTION('ref_axis',(1.,0.,0.));
#18348=DIRECTION('',(1.,0.,0.));
#18349=DIRECTION('',(0.,0.707106781186548,0.707106781186548));
#18350=DIRECTION('center_axis',(0.,0.,-1.));
#18351=DIRECTION('ref_axis',(0.707106781186547,-0.707106781186547,0.));
#18352=DIRECTION('center_axis',(0.,0.,1.));
#18353=DIRECTION('ref_axis',(0.707106781186548,-0.707106781186548,0.));
#18354=DIRECTION('center_axis',(0.,-0.707106781186548,0.707106781186548));
#18355=DIRECTION('ref_axis',(1.,0.,0.));
#18356=DIRECTION('',(0.,0.707106781186548,0.707106781186548));
#18357=DIRECTION('center_axis',(0.,0.,1.));
#18358=DIRECTION('ref_axis',(0.,-1.,0.));
#18359=DIRECTION('',(0.,-0.707106781186548,0.707106781186548));
#18360=DIRECTION('center_axis',(0.,0.707106781186548,0.707106781186548));
#18361=DIRECTION('ref_axis',(1.,0.,0.));
#18362=DIRECTION('center_axis',(0.,0.,1.));
#18363=DIRECTION('ref_axis',(0.,1.,0.));
#18364=DIRECTION('center_axis',(0.,0.,-1.));
#18365=DIRECTION('ref_axis',(0.,1.,0.));
#18366=DIRECTION('center_axis',(0.,0.,1.));
#18367=DIRECTION('ref_axis',(0.,-1.,0.));
#18368=DIRECTION('',(0.,-0.707106781186548,0.707106781186548));
#18369=DIRECTION('center_axis',(0.,0.707106781186548,0.707106781186548));
#18370=DIRECTION('ref_axis',(1.,0.,0.));
#18371=DIRECTION('center_axis',(0.,0.,1.));
#18372=DIRECTION('ref_axis',(0.,1.,0.));
#18373=DIRECTION('center_axis',(0.,0.,-1.));
#18374=DIRECTION('ref_axis',(0.,1.,0.));
#18375=DIRECTION('center_axis',(0.,0.,1.));
#18376=DIRECTION('ref_axis',(0.707106781186547,-0.707106781186547,0.));
#18377=DIRECTION('',(0.,0.,-1.));
#18378=DIRECTION('center_axis',(0.,-1.,0.));
#18379=DIRECTION('ref_axis',(1.,0.,0.));
#18380=DIRECTION('',(0.,0.,1.));
#18381=DIRECTION('center_axis',(0.,0.,1.));
#18382=DIRECTION('ref_axis',(-0.707106781186547,-0.707106781186547,0.));
#18383=DIRECTION('center_axis',(0.,-1.,0.));
#18384=DIRECTION('ref_axis',(-1.,0.,0.));
#18385=DIRECTION('',(0.,0.,-1.));
#18386=DIRECTION('center_axis',(0.,0.,-1.));
#18387=DIRECTION('ref_axis',(0.,1.,0.));
#18388=DIRECTION('center_axis',(0.,-1.,0.));
#18389=DIRECTION('ref_axis',(-1.,0.,0.));
#18390=DIRECTION('',(0.,0.,-1.));
#18391=DIRECTION('center_axis',(0.,1.,0.));
#18392=DIRECTION('ref_axis',(1.,0.,0.));
#18393=DIRECTION('',(0.,0.,-1.));
#18394=DIRECTION('center_axis',(0.,0.,-1.));
#18395=DIRECTION('ref_axis',(0.,1.,0.));
#18396=DIRECTION('axis',(0.,0.,1.));
#18397=DIRECTION('refdir',(1.,0.,0.));
#18398=DIRECTION('center_axis',(-1.,0.,0.));
#18399=DIRECTION('ref_axis',(0.,0.,1.));
#18400=DIRECTION('center_axis',(-1.,0.,0.));
#18401=DIRECTION('ref_axis',(0.,0.,1.));
#18402=DIRECTION('center_axis',(1.,0.,0.));
#18403=DIRECTION('ref_axis',(0.,0.,1.));
#18404=DIRECTION('center_axis',(-1.,0.,0.));
#18405=DIRECTION('ref_axis',(0.,0.,1.));
#18406=DIRECTION('center_axis',(-1.,0.,0.));
#18407=DIRECTION('ref_axis',(0.,0.,1.));
#18408=DIRECTION('',(-0.707106781186547,-8.65956056235493E-17,-0.707106781186548));
#18409=DIRECTION('center_axis',(-1.,0.,0.));
#18410=DIRECTION('ref_axis',(0.,0.,1.));
#18411=DIRECTION('center_axis',(-1.,0.,0.));
#18412=DIRECTION('ref_axis',(0.,0.,1.));
#18413=DIRECTION('',(-1.,0.,0.));
#18414=DIRECTION('center_axis',(-1.,0.,0.));
#18415=DIRECTION('ref_axis',(0.,0.,1.));
#18416=DIRECTION('center_axis',(0.,-1.,0.));
#18417=DIRECTION('ref_axis',(0.,0.,1.));
#18418=DIRECTION('center_axis',(0.,1.,0.));
#18419=DIRECTION('ref_axis',(1.,0.,0.));
#18420=DIRECTION('',(8.65956056235493E-17,0.707106781186547,0.707106781186548));
#18421=DIRECTION('center_axis',(0.,-1.,0.));
#18422=DIRECTION('ref_axis',(0.,0.,1.));
#18423=DIRECTION('center_axis',(0.,-1.,0.));
#18424=DIRECTION('ref_axis',(0.,0.,-1.));
#18425=DIRECTION('center_axis',(0.,1.,0.));
#18426=DIRECTION('ref_axis',(0.,0.,1.));
#18427=DIRECTION('center_axis',(0.,1.,0.));
#18428=DIRECTION('ref_axis',(0.,0.,1.));
#18429=DIRECTION('',(0.,1.,0.));
#18430=DIRECTION('center_axis',(1.,0.,0.));
#18431=DIRECTION('ref_axis',(0.,0.,-1.));
#18432=DIRECTION('',(0.,0.,1.));
#18433=DIRECTION('center_axis',(1.,0.,0.));
#18434=DIRECTION('ref_axis',(0.,0.,-1.));
#18435=DIRECTION('',(0.,0.,-1.));
#18436=DIRECTION('center_axis',(-1.,0.,0.));
#18437=DIRECTION('ref_axis',(0.,0.,1.));
#18438=DIRECTION('',(-1.,0.,0.));
#18439=DIRECTION('center_axis',(0.,1.,0.));
#18440=DIRECTION('ref_axis',(0.,0.,1.));
#18441=DIRECTION('',(0.,0.,1.));
#18442=DIRECTION('center_axis',(0.,1.,0.));
#18443=DIRECTION('ref_axis',(1.,0.,0.));
#18444=DIRECTION('center_axis',(0.,1.,0.));
#18445=DIRECTION('ref_axis',(0.,0.,1.));
#18446=DIRECTION('',(0.,1.,0.));
#18447=DIRECTION('center_axis',(0.,1.,0.));
#18448=DIRECTION('ref_axis',(1.,0.,0.));
#18449=DIRECTION('center_axis',(0.,1.,0.));
#18450=DIRECTION('ref_axis',(0.,0.,1.));
#18451=DIRECTION('',(0.,0.,-1.));
#18452=DIRECTION('center_axis',(0.,0.,-1.));
#18453=DIRECTION('ref_axis',(-1.,0.,0.));
#18454=DIRECTION('center_axis',(0.,0.,1.));
#18455=DIRECTION('ref_axis',(1.,0.,0.));
#18456=DIRECTION('center_axis',(0.,0.,1.));
#18457=DIRECTION('ref_axis',(1.,0.,0.));
#18458=DIRECTION('center_axis',(0.,0.,1.));
#18459=DIRECTION('ref_axis',(1.,0.,0.));
#18460=DIRECTION('',(0.707106781186548,8.65956056235494E-17,-0.707106781186547));
#18461=DIRECTION('center_axis',(0.,0.,1.));
#18462=DIRECTION('ref_axis',(1.,0.,0.));
#18463=DIRECTION('center_axis',(0.,0.,1.));
#18464=DIRECTION('ref_axis',(1.,0.,0.));
#18465=DIRECTION('',(0.,0.,-1.));
#18466=DIRECTION('center_axis',(0.,0.,-1.));
#18467=DIRECTION('ref_axis',(-1.,0.,0.));
#18468=DIRECTION('center_axis',(0.,0.,1.));
#18469=DIRECTION('ref_axis',(1.,0.,0.));
#18470=DIRECTION('center_axis',(0.,0.,1.));
#18471=DIRECTION('ref_axis',(1.,0.,0.));
#18472=DIRECTION('center_axis',(0.,0.,1.));
#18473=DIRECTION('ref_axis',(1.,0.,0.));
#18474=DIRECTION('',(0.707106781186546,8.65956056235491E-17,-0.707106781186549));
#18475=DIRECTION('center_axis',(0.,0.,1.));
#18476=DIRECTION('ref_axis',(1.,0.,0.));
#18477=DIRECTION('center_axis',(0.,0.,1.));
#18478=DIRECTION('ref_axis',(1.,0.,0.));
#18479=DIRECTION('',(0.,0.,-1.));
#18480=DIRECTION('',(0.,0.,-1.));
#18481=DIRECTION('center_axis',(0.,0.,-1.));
#18482=DIRECTION('ref_axis',(1.,0.,0.));
#18483=DIRECTION('center_axis',(0.,0.,1.));
#18484=DIRECTION('ref_axis',(1.,0.,0.));
#18485=DIRECTION('',(-0.707106781186547,-8.65956056235493E-17,-0.707106781186547));
#18486=DIRECTION('center_axis',(0.,0.,1.));
#18487=DIRECTION('ref_axis',(1.,0.,0.));
#18488=DIRECTION('center_axis',(0.,0.,1.));
#18489=DIRECTION('ref_axis',(1.,0.,0.));
#18490=DIRECTION('center_axis',(0.,0.,1.));
#18491=DIRECTION('ref_axis',(1.,0.,0.));
#18492=DIRECTION('',(0.707106781186549,8.65956056235495E-17,-0.707106781186546));
#18493=DIRECTION('center_axis',(0.,0.,1.));
#18494=DIRECTION('ref_axis',(1.,0.,0.));
#18495=DIRECTION('center_axis',(0.,0.,1.));
#18496=DIRECTION('ref_axis',(1.,0.,0.));
#18497=DIRECTION('',(0.,0.,-1.));
#18498=DIRECTION('',(0.,0.,-1.));
#18499=DIRECTION('center_axis',(0.,0.,1.));
#18500=DIRECTION('ref_axis',(1.,0.,0.));
#18501=DIRECTION('center_axis',(0.,0.,1.));
#18502=DIRECTION('ref_axis',(1.,0.,0.));
#18503=DIRECTION('axis',(0.,0.,1.));
#18504=DIRECTION('refdir',(1.,0.,0.));
#18505=DIRECTION('center_axis',(0.,-1.93747046180099E-15,-1.));
#18506=DIRECTION('ref_axis',(-1.,-3.18304947217744E-17,0.));
#18507=DIRECTION('center_axis',(0.,0.,-1.));
#18508=DIRECTION('ref_axis',(-1.,0.,0.));
#18509=DIRECTION('',(0.923879532511291,-5.98887692616032E-16,-0.38268343236508));
#18510=DIRECTION('center_axis',(0.,0.,1.));
#18511=DIRECTION('ref_axis',(-1.,-6.12323399573677E-17,0.));
#18512=DIRECTION('center_axis',(0.,0.,1.));
#18513=DIRECTION('ref_axis',(-1.,-6.12323399573677E-17,0.));
#18514=DIRECTION('center_axis',(0.,0.,-1.));
#18515=DIRECTION('ref_axis',(1.,0.,0.));
#18516=DIRECTION('',(-0.707106781186548,-8.65956056235494E-17,-0.707106781186547));
#18517=DIRECTION('center_axis',(0.,0.,-1.));
#18518=DIRECTION('ref_axis',(-1.,-6.12323399573677E-17,0.));
#18519=DIRECTION('center_axis',(0.,0.,-1.));
#18520=DIRECTION('ref_axis',(-1.,-6.12323399573677E-17,0.));
#18521=DIRECTION('center_axis',(0.,0.,1.));
#18522=DIRECTION('ref_axis',(1.,0.,0.));
#18523=DIRECTION('center_axis',(0.,8.11581801128163E-16,-1.));
#18524=DIRECTION('ref_axis',(-1.,-3.01451275783686E-17,0.));
#18525=DIRECTION('',(0.382683432365092,8.08205059964992E-16,-0.923879532511286));
#18526=DIRECTION('center_axis',(0.,0.,1.));
#18527=DIRECTION('ref_axis',(-1.,0.,0.));
#18528=DIRECTION('center_axis',(0.,0.,1.));
#18529=DIRECTION('ref_axis',(-1.,0.,0.));
#18530=DIRECTION('center_axis',(0.,0.,1.));
#18531=DIRECTION('ref_axis',(1.,0.,0.));
#18532=DIRECTION('',(0.,0.,-1.));
#18533=DIRECTION('center_axis',(0.,0.,-1.));
#18534=DIRECTION('ref_axis',(-1.,0.,0.));
#18535=DIRECTION('center_axis',(0.,0.,-1.));
#18536=DIRECTION('ref_axis',(-1.,0.,0.));
#18537=DIRECTION('center_axis',(0.,8.11581801128149E-16,1.));
#18538=DIRECTION('ref_axis',(-1.,-3.01451275783686E-17,0.));
#18539=DIRECTION('',(-0.382683432365084,-8.0820505996498E-16,-0.923879532511289));
#18540=DIRECTION('center_axis',(0.,0.,1.));
#18541=DIRECTION('ref_axis',(-1.,-6.12323399573677E-17,0.));
#18542=DIRECTION('center_axis',(0.,0.,1.));
#18543=DIRECTION('ref_axis',(-1.,-6.12323399573677E-17,0.));
#18544=DIRECTION('center_axis',(0.,0.,1.));
#18545=DIRECTION('ref_axis',(1.,0.,0.));
#18546=DIRECTION('',(0.707106781186547,8.65956056235492E-17,-0.707106781186548));
#18547=DIRECTION('center_axis',(0.,0.,-1.));
#18548=DIRECTION('ref_axis',(-1.,-6.12323399573676E-17,0.));
#18549=DIRECTION('center_axis',(0.,0.,-1.));
#18550=DIRECTION('ref_axis',(-1.,-6.12323399573676E-17,0.));
#18551=DIRECTION('center_axis',(0.,-1.93747046180093E-15,1.));
#18552=DIRECTION('ref_axis',(-1.,-3.18304947217744E-17,0.));
#18553=DIRECTION('',(-0.923879532511287,5.98887692616029E-16,-0.38268343236509));
#18554=DIRECTION('center_axis',(0.,0.,1.));
#18555=DIRECTION('ref_axis',(-1.,0.,0.));
#18556=DIRECTION('center_axis',(0.,0.,-1.));
#18557=DIRECTION('ref_axis',(-1.,0.,0.));
#18558=DIRECTION('axis',(0.,0.,1.));
#18559=DIRECTION('refdir',(1.,0.,0.));
#18560=DIRECTION('center_axis',(0.923879532511287,0.382683432365089,0.));
#18561=DIRECTION('ref_axis',(0.,0.,-1.));
#18562=DIRECTION('',(-0.336556770590777,0.812519920068747,0.475963149477966));
#18563=DIRECTION('',(0.,0.,1.));
#18564=DIRECTION('',(0.336556770590775,-0.812519920068743,0.475963149477973));
#18565=DIRECTION('',(0.28108463771482,-0.678598344545848,-0.678598344545846));
#18566=DIRECTION('',(0.,0.,-1.));
#18567=DIRECTION('',(-0.281084637714818,0.678598344545843,-0.678598344545852));
#18568=DIRECTION('center_axis',(0.923879532511287,0.,0.38268343236509));
#18569=DIRECTION('ref_axis',(0.38268343236509,0.,-0.923879532511287));
#18570=DIRECTION('',(-0.33655677059078,-0.475963149477958,0.81251992006875));
#18571=DIRECTION('',(0.,-1.,0.));
#18572=DIRECTION('',(0.33655677059078,-0.475963149477958,-0.81251992006875));
#18573=DIRECTION('',(0.357406744336593,0.357406744336595,-0.862856209461016));
#18574=DIRECTION('',(0.,1.,0.));
#18575=DIRECTION('center_axis',(0.57735026918963,0.577350269189628,0.57735026918962));
#18576=DIRECTION('ref_axis',(0.707106781186541,0.,-0.707106781186554));
#18577=DIRECTION('',(0.707106781186546,-0.707106781186549,0.));
#18578=DIRECTION('',(0.812519920068742,-0.336556770590782,-0.47596314947797));
#18579=DIRECTION('',(0.475963149477956,0.336556770590781,-0.812519920068751));
#18580=DIRECTION('',(0.,0.707106781186543,-0.707106781186552));
#18581=DIRECTION('',(-0.475963149477964,0.812519920068745,-0.336556770590783));
#18582=DIRECTION('',(-0.81251992006874,0.475963149477997,0.336556770590751));
#18583=DIRECTION('',(-0.707106781186541,0.,0.707106781186554));
#18584=DIRECTION('center_axis',(0.707106781186549,0.707106781186546,0.));
#18585=DIRECTION('ref_axis',(0.,0.,-1.));
#18586=DIRECTION('',(-0.707106781186546,0.707106781186549,0.));
#18587=DIRECTION('',(0.,0.,-1.));
#18588=DIRECTION('center_axis',(0.923879532511289,0.,-0.382683432365084));
#18589=DIRECTION('ref_axis',(-0.382683432365084,0.,-0.923879532511289));
#18590=DIRECTION('',(0.,-1.,0.));
#18591=DIRECTION('',(-0.357406744336588,-0.35740674433659,-0.86285620946102));
#18592=DIRECTION('',(-0.336556770590771,0.475963149477975,-0.812519920068744));
#18593=DIRECTION('',(0.,1.,0.));
#18594=DIRECTION('',(0.336556770590771,0.475963149477975,0.812519920068744));
#18595=DIRECTION('center_axis',(1.,0.,0.));
#18596=DIRECTION('ref_axis',(0.,0.,-1.));
#18597=DIRECTION('',(0.,0.,1.));
#18598=DIRECTION('center_axis',(0.577350269189627,0.577350269189624,-0.577350269189627));
#18599=DIRECTION('ref_axis',(-0.707106781186548,0.,-0.707106781186548));
#18600=DIRECTION('',(0.707106781186548,0.,0.707106781186548));
#18601=DIRECTION('',(0.812519920068745,-0.475963149477963,0.336556770590785));
#18602=DIRECTION('',(0.475963149477962,-0.812519920068747,-0.336556770590781));
#18603=DIRECTION('',(0.,-0.707106781186549,-0.707106781186546));
#18604=DIRECTION('',(-0.475963149477966,-0.336556770590781,-0.812519920068745));
#18605=DIRECTION('',(-0.812519920068746,0.336556770590784,-0.475963149477963));
#18606=DIRECTION('center_axis',(0.707106781186549,-0.707106781186546,0.));
#18607=DIRECTION('ref_axis',(0.,0.,-1.));
#18608=DIRECTION('',(-0.707106781186546,-0.707106781186549,0.));
#18609=DIRECTION('',(0.,0.,1.));
#18610=DIRECTION('',(0.707106781186546,0.707106781186549,0.));
#18611=DIRECTION('center_axis',(0.57735026918963,-0.577350269189628,0.57735026918962));
#18612=DIRECTION('ref_axis',(0.707106781186541,0.,-0.707106781186554));
#18613=DIRECTION('',(0.707106781186541,0.,-0.707106781186554));
#18614=DIRECTION('',(0.81251992006874,0.475963149477997,-0.336556770590751));
#18615=DIRECTION('',(0.475963149477962,0.812519920068746,0.336556770590786));
#18616=DIRECTION('',(0.,0.707106781186543,0.707106781186552));
#18617=DIRECTION('',(-0.475963149477956,0.336556770590782,0.812519920068751));
#18618=DIRECTION('',(-0.812519920068742,-0.336556770590782,0.475963149477971));
#18619=DIRECTION('center_axis',(0.,0.382683432365093,-0.923879532511286));
#18620=DIRECTION('ref_axis',(-1.,0.,0.));
#18621=DIRECTION('',(0.475963149477956,0.81251992006875,0.336556770590782));
#18622=DIRECTION('',(1.,0.,0.));
#18623=DIRECTION('',(-0.678598344545842,-0.67859834454585,-0.281084637714824));
#18624=DIRECTION('',(-1.,0.,0.));
#18625=DIRECTION('',(-0.678598344545842,0.67859834454585,0.281084637714824));
#18626=DIRECTION('center_axis',(-0.382683432365097,0.,-0.923879532511284));
#18627=DIRECTION('ref_axis',(-0.923879532511284,0.,0.382683432365097));
#18628=DIRECTION('',(0.,-1.,0.));
#18629=DIRECTION('',(-0.678598344545841,-0.678598344545852,0.281084637714824));
#18630=DIRECTION('',(-0.81251992006874,0.475963149477974,0.336556770590782));
#18631=DIRECTION('',(0.,1.,0.));
#18632=DIRECTION('',(0.81251992006874,0.475963149477974,-0.336556770590782));
#18633=DIRECTION('center_axis',(0.,0.,-1.));
#18634=DIRECTION('ref_axis',(-1.,0.,0.));
#18635=DIRECTION('',(0.,1.,0.));
#18636=DIRECTION('',(1.,0.,0.));
#18637=DIRECTION('center_axis',(0.382683432365097,0.,-0.923879532511284));
#18638=DIRECTION('ref_axis',(-0.923879532511284,0.,-0.382683432365097));
#18639=DIRECTION('',(0.,-1.,0.));
#18640=DIRECTION('',(-0.812519920068745,-0.475963149477963,-0.336556770590785));
#18641=DIRECTION('',(-0.678598344545841,0.678598344545852,-0.281084637714824));
#18642=DIRECTION('center_axis',(0.,0.707106781186546,-0.707106781186549));
#18643=DIRECTION('ref_axis',(-1.,0.,0.));
#18644=DIRECTION('',(0.,0.707106781186549,0.707106781186546));
#18645=DIRECTION('',(-1.,0.,0.));
#18646=DIRECTION('center_axis',(-0.577350269189634,0.577350269189621,-0.577350269189623));
#18647=DIRECTION('ref_axis',(-0.707106781186541,0.,0.707106781186554));
#18648=DIRECTION('',(0.707106781186541,0.,-0.707106781186554));
#18649=DIRECTION('',(0.336556770590786,-0.475963149477958,-0.812519920068748));
#18650=DIRECTION('',(-0.336556770590778,-0.812519920068749,-0.475963149477962));
#18651=DIRECTION('',(-0.707106781186546,-0.707106781186549,1.25607396694702E-14));
#18652=DIRECTION('',(-0.81251992006874,-0.336556770590781,0.475963149477975));
#18653=DIRECTION('',(-0.475963149477959,0.336556770590782,0.812519920068749));
#18654=DIRECTION('center_axis',(-0.923879532511287,0.382683432365089,0.));
#18655=DIRECTION('ref_axis',(0.,0.,1.));
#18656=DIRECTION('',(0.336556770590775,0.812519920068743,-0.475963149477973));
#18657=DIRECTION('',(0.,0.,-1.));
#18658=DIRECTION('',(-0.281084637714823,-0.678598344545855,0.678598344545838));
#18659=DIRECTION('',(0.,0.,1.));
#18660=DIRECTION('',(0.28108463771483,0.678598344545872,0.678598344545818));
#18661=DIRECTION('center_axis',(-0.923879532511276,0.,0.382683432365115));
#18662=DIRECTION('ref_axis',(0.382683432365115,0.,0.923879532511276));
#18663=DIRECTION('',(0.,-1.,0.));
#18664=DIRECTION('',(0.357406744336614,-0.357406744336615,0.862856209460999));
#18665=DIRECTION('',(0.336556770590807,0.475963149477934,0.812519920068753));
#18666=DIRECTION('',(0.,1.,0.));
#18667=DIRECTION('',(-0.336556770590807,0.475963149477934,-0.812519920068753));
#18668=DIRECTION('center_axis',(-1.,0.,0.));
#18669=DIRECTION('ref_axis',(0.,0.,1.));
#18670=DIRECTION('',(0.,1.,0.));
#18671=DIRECTION('',(0.,0.,-1.));
#18672=DIRECTION('center_axis',(-0.923879532511284,0.,-0.382683432365097));
#18673=DIRECTION('ref_axis',(-0.382683432365097,0.,0.923879532511284));
#18674=DIRECTION('',(0.,-1.,0.));
#18675=DIRECTION('',(-0.336556770590786,-0.475963149477958,0.812519920068748));
#18676=DIRECTION('',(-0.357406744336599,0.3574067443366,0.862856209461012));
#18677=DIRECTION('center_axis',(-0.707106781186549,-0.707106781186546,0.));
#18678=DIRECTION('ref_axis',(0.,0.,1.));
#18679=DIRECTION('',(0.707106781186546,-0.707106781186549,-1.25607396694702E-14));
#18680=DIRECTION('',(0.,0.,-1.));
#18681=DIRECTION('',(-0.707106781186546,0.707106781186549,0.));
#18682=DIRECTION('center_axis',(-0.577350269189634,-0.577350269189621,-0.577350269189623));
#18683=DIRECTION('ref_axis',(-0.707106781186541,0.,0.707106781186554));
#18684=DIRECTION('',(-0.475963149477957,0.81251992006875,-0.336556770590781));
#18685=DIRECTION('',(0.,0.707106781186549,-0.707106781186546));
#18686=DIRECTION('',(0.475963149477953,0.33655677059079,-0.812519920068749));
#18687=DIRECTION('',(0.81251992006874,-0.336556770590781,-0.475963149477975));
#18688=DIRECTION('',(-0.707106781186541,0.,0.707106781186554));
#18689=DIRECTION('center_axis',(-0.57735026918963,0.577350269189628,0.57735026918962));
#18690=DIRECTION('ref_axis',(0.707106781186541,0.,0.707106781186554));
#18691=DIRECTION('',(-0.707106781186541,0.,-0.707106781186554));
#18692=DIRECTION('',(-0.81251992006874,-0.475963149477994,-0.336556770590754));
#18693=DIRECTION('',(-0.475963149477964,-0.812519920068745,0.336556770590783));
#18694=DIRECTION('',(0.,-0.707106781186543,0.707106781186552));
#18695=DIRECTION('',(0.475963149477957,-0.336556770590781,0.812519920068751));
#18696=DIRECTION('',(0.812519920068742,0.336556770590782,0.47596314947797));
#18697=DIRECTION('',(0.707106781186546,0.707106781186549,0.));
#18698=DIRECTION('center_axis',(-0.707106781186554,0.,0.707106781186541));
#18699=DIRECTION('ref_axis',(0.707106781186541,0.,0.707106781186554));
#18700=DIRECTION('',(0.707106781186541,0.,0.707106781186554));
#18701=DIRECTION('',(0.,-1.,0.));
#18702=DIRECTION('center_axis',(-0.57735026918963,-0.577350269189628,0.57735026918962));
#18703=DIRECTION('ref_axis',(0.707106781186541,0.,0.707106781186554));
#18704=DIRECTION('',(-0.812519920068742,0.336556770590782,-0.475963149477971));
#18705=DIRECTION('',(-0.475963149477956,-0.336556770590782,-0.812519920068751));
#18706=DIRECTION('',(0.,-0.707106781186543,-0.707106781186552));
#18707=DIRECTION('',(0.475963149477962,-0.812519920068746,-0.336556770590786));
#18708=DIRECTION('',(0.81251992006874,-0.475963149477994,0.336556770590754));
#18709=DIRECTION('center_axis',(0.,0.382683432365095,0.923879532511284));
#18710=DIRECTION('ref_axis',(1.,0.,0.));
#18711=DIRECTION('',(-1.,0.,0.));
#18712=DIRECTION('',(0.678598344545875,-0.678598344545821,0.281084637714814));
#18713=DIRECTION('',(1.,0.,0.));
#18714=DIRECTION('',(0.678598344545879,0.678598344545818,-0.281084637714813));
#18715=DIRECTION('center_axis',(-0.382683432365069,0.,0.923879532511295));
#18716=DIRECTION('ref_axis',(0.923879532511295,0.,0.382683432365069));
#18717=DIRECTION('',(0.678598344545878,0.678598344545818,0.281084637714815));
#18718=DIRECTION('',(0.,1.,0.));
#18719=DIRECTION('center_axis',(0.,0.707106781186552,0.707106781186543));
#18720=DIRECTION('ref_axis',(1.,0.,0.));
#18721=DIRECTION('',(1.,0.,0.));
#18722=DIRECTION('center_axis',(0.382683432365067,0.,0.923879532511296));
#18723=DIRECTION('ref_axis',(0.923879532511296,0.,-0.382683432365067));
#18724=DIRECTION('',(0.,-1.,0.));
#18725=DIRECTION('',(0.678598344545881,-0.678598344545815,-0.281084637714814));
#18726=DIRECTION('',(0.,1.,0.));
#18727=DIRECTION('center_axis',(0.,-0.382683432365098,0.923879532511283));
#18728=DIRECTION('ref_axis',(1.,0.,0.));
#18729=DIRECTION('',(-1.,0.,0.));
#18730=DIRECTION('',(1.,0.,0.));
#18731=DIRECTION('center_axis',(0.,0.,1.));
#18732=DIRECTION('ref_axis',(1.,0.,0.));
#18733=DIRECTION('center_axis',(-0.382683432365096,0.923879532511284,0.));
#18734=DIRECTION('ref_axis',(0.,0.,1.));
#18735=DIRECTION('',(0.,0.,1.));
#18736=DIRECTION('',(0.678598344545842,0.281084637714823,-0.678598344545851));
#18737=DIRECTION('',(0.,0.,-1.));
#18738=DIRECTION('',(-0.678598344545843,-0.281084637714824,-0.678598344545849));
#18739=DIRECTION('center_axis',(0.,0.923879532511286,0.382683432365091));
#18740=DIRECTION('ref_axis',(0.,-0.382683432365091,0.923879532511286));
#18741=DIRECTION('',(0.678598344545842,-0.281084637714823,0.678598344545851));
#18742=DIRECTION('',(-1.,0.,0.));
#18743=DIRECTION('center_axis',(-0.707106781186549,0.707106781186546,0.));
#18744=DIRECTION('ref_axis',(0.,0.,1.));
#18745=DIRECTION('center_axis',(0.382683432365096,0.923879532511284,0.));
#18746=DIRECTION('ref_axis',(0.,0.,1.));
#18747=DIRECTION('',(-0.678598344545843,0.281084637714824,0.678598344545849));
#18748=DIRECTION('',(0.,0.,1.));
#18749=DIRECTION('center_axis',(0.,1.,0.));
#18750=DIRECTION('ref_axis',(0.,0.,1.));
#18751=DIRECTION('',(1.,0.,0.));
#18752=DIRECTION('center_axis',(0.,1.,0.));
#18753=DIRECTION('ref_axis',(0.,0.,1.));
#18754=DIRECTION('center_axis',(0.,1.,0.));
#18755=DIRECTION('ref_axis',(0.,0.,1.));
#18756=DIRECTION('center_axis',(0.,1.,0.));
#18757=DIRECTION('ref_axis',(0.,0.,1.));
#18758=DIRECTION('center_axis',(0.,1.,0.));
#18759=DIRECTION('ref_axis',(0.,0.,1.));
#18760=DIRECTION('center_axis',(0.,1.,0.));
#18761=DIRECTION('ref_axis',(0.,0.,1.));
#18762=DIRECTION('center_axis',(0.,1.,0.));
#18763=DIRECTION('ref_axis',(1.,0.,0.));
#18764=DIRECTION('center_axis',(0.,0.923879532511285,-0.382683432365093));
#18765=DIRECTION('ref_axis',(0.,0.382683432365093,0.923879532511285));
#18766=DIRECTION('center_axis',(0.,-0.707106781186552,0.707106781186543));
#18767=DIRECTION('ref_axis',(1.,0.,0.));
#18768=DIRECTION('',(-1.,0.,0.));
#18769=DIRECTION('center_axis',(0.,-0.382683432365092,-0.923879532511286));
#18770=DIRECTION('ref_axis',(-1.,0.,0.));
#18771=DIRECTION('',(-0.475963149477963,-0.812519920068747,0.33655677059078));
#18772=DIRECTION('',(-1.,0.,0.));
#18773=DIRECTION('center_axis',(0.,-0.707106781186546,-0.707106781186549));
#18774=DIRECTION('ref_axis',(-1.,0.,0.));
#18775=DIRECTION('',(0.,-0.707106781186549,0.707106781186546));
#18776=DIRECTION('',(1.,0.,0.));
#18777=DIRECTION('center_axis',(0.577350269189627,-0.577350269189624,-0.577350269189627));
#18778=DIRECTION('ref_axis',(-0.707106781186548,0.,-0.707106781186548));
#18779=DIRECTION('',(0.812519920068745,0.336556770590783,0.475963149477964));
#18780=DIRECTION('',(0.475963149477959,-0.336556770590788,0.812519920068746));
#18781=DIRECTION('',(-0.707106781186548,0.,-0.707106781186548));
#18782=DIRECTION('center_axis',(2.16784530188846E-15,-1.,0.));
#18783=DIRECTION('ref_axis',(-1.,0.,0.));
#18784=DIRECTION('center_axis',(0.,1.,0.));
#18785=DIRECTION('ref_axis',(-1.,0.,0.));
#18786=DIRECTION('center_axis',(0.,1.,0.));
#18787=DIRECTION('ref_axis',(-1.,0.,0.));
#18788=DIRECTION('',(0.38268343236509,-0.923879532511287,-4.68652040532627E-17));
#18789=DIRECTION('center_axis',(0.,-1.,-3.96079183235886E-16));
#18790=DIRECTION('ref_axis',(-1.,0.,0.));
#18791=DIRECTION('center_axis',(0.,-1.,-3.96079183235886E-16));
#18792=DIRECTION('ref_axis',(-1.,0.,0.));
#18793=DIRECTION('center_axis',(0.,-1.,0.));
#18794=DIRECTION('ref_axis',(1.,0.,0.));
#18795=DIRECTION('center_axis',(0.,-1.,0.));
#18796=DIRECTION('ref_axis',(-1.,0.,0.));
#18797=DIRECTION('center_axis',(0.,-1.,0.));
#18798=DIRECTION('ref_axis',(-1.,0.,0.));
#18799=DIRECTION('',(0.,-1.,0.));
#18800=DIRECTION('center_axis',(0.,-1.,0.));
#18801=DIRECTION('ref_axis',(1.,0.,0.));
#18802=DIRECTION('',(-0.707106781186548,-0.707106781186548,-8.65956056235493E-17));
#18803=DIRECTION('center_axis',(-9.83554226541497E-17,1.,3.93421690616599E-16));
#18804=DIRECTION('ref_axis',(1.,9.83554226541497E-17,0.));
#18805=DIRECTION('center_axis',(0.,1.,0.));
#18806=DIRECTION('ref_axis',(-1.,0.,0.));
#18807=DIRECTION('center_axis',(0.,1.,0.));
#18808=DIRECTION('ref_axis',(-1.,0.,0.));
#18809=DIRECTION('',(-0.707106781186548,-0.707106781186548,8.65956056235493E-17));
#18810=DIRECTION('center_axis',(0.,-1.,0.));
#18811=DIRECTION('ref_axis',(0.,0.,-1.));
#18812=DIRECTION('center_axis',(0.,-1.,0.));
#18813=DIRECTION('ref_axis',(1.,0.,0.));
#18814=DIRECTION('center_axis',(0.,1.,0.));
#18815=DIRECTION('ref_axis',(-1.,0.,0.));
#18816=DIRECTION('center_axis',(0.,1.,0.));
#18817=DIRECTION('ref_axis',(-1.,0.,0.));
#18818=DIRECTION('',(-0.707106781186547,-0.707106781186547,8.65956056235493E-17));
#18819=DIRECTION('center_axis',(0.,-1.,0.));
#18820=DIRECTION('ref_axis',(-1.,0.,0.));
#18821=DIRECTION('center_axis',(0.,-1.,0.));
#18822=DIRECTION('ref_axis',(-1.,0.,0.));
#18823=DIRECTION('center_axis',(0.,-1.,0.));
#18824=DIRECTION('ref_axis',(0.,0.,-1.));
#18825=DIRECTION('center_axis',(0.,-1.,0.));
#18826=DIRECTION('ref_axis',(1.,0.,0.));
#18827=DIRECTION('center_axis',(0.,-1.,0.));
#18828=DIRECTION('ref_axis',(1.,0.,0.));
#18829=DIRECTION('',(0.,-1.,0.));
#18830=DIRECTION('center_axis',(0.,1.,0.));
#18831=DIRECTION('ref_axis',(1.,0.,0.));
#18832=DIRECTION('',(0.707106781186548,-0.707106781186547,-8.65956056235494E-17));
#18833=DIRECTION('center_axis',(0.,-1.,0.));
#18834=DIRECTION('ref_axis',(1.,0.,0.));
#18835=DIRECTION('center_axis',(0.,-1.,0.));
#18836=DIRECTION('ref_axis',(1.,0.,0.));
#18837=DIRECTION('',(0.,-1.,0.));
#18838=DIRECTION('center_axis',(0.,1.,0.));
#18839=DIRECTION('ref_axis',(0.,0.,1.));
#18840=DIRECTION('',(8.65956056235484E-17,-0.707106781186555,0.70710678118654));
#18841=DIRECTION('center_axis',(0.,-1.,0.));
#18842=DIRECTION('ref_axis',(0.,0.,1.));
#18843=DIRECTION('center_axis',(0.,1.,0.));
#18844=DIRECTION('ref_axis',(0.,0.,1.));
#18845=DIRECTION('center_axis',(0.,1.,0.));
#18846=DIRECTION('ref_axis',(0.,0.,-1.));
#18847=DIRECTION('center_axis',(0.,1.,0.));
#18848=DIRECTION('ref_axis',(0.,0.,-1.));
#18849=DIRECTION('',(0.,1.,0.));
#18850=DIRECTION('center_axis',(0.,-1.,0.));
#18851=DIRECTION('ref_axis',(0.,0.,-1.));
#18852=DIRECTION('center_axis',(0.,-1.,0.));
#18853=DIRECTION('ref_axis',(0.,0.,-1.));
#18854=DIRECTION('',(8.65956056235484E-17,0.707106781186555,-0.70710678118654));
#18855=DIRECTION('center_axis',(0.,1.,0.));
#18856=DIRECTION('ref_axis',(0.,0.,1.));
#18857=DIRECTION('center_axis',(0.,1.,0.));
#18858=DIRECTION('ref_axis',(1.,0.,0.));
#18859=DIRECTION('center_axis',(0.,1.,0.));
#18860=DIRECTION('ref_axis',(0.,0.,1.));
#18861=DIRECTION('',(8.65956056235497E-17,-0.707106781186545,0.70710678118655));
#18862=DIRECTION('center_axis',(0.,-1.,0.));
#18863=DIRECTION('ref_axis',(0.,0.,1.));
#18864=DIRECTION('center_axis',(0.,1.,0.));
#18865=DIRECTION('ref_axis',(0.,0.,1.));
#18866=DIRECTION('center_axis',(0.,1.,0.));
#18867=DIRECTION('ref_axis',(0.,0.,-1.));
#18868=DIRECTION('center_axis',(0.,1.,0.));
#18869=DIRECTION('ref_axis',(0.,0.,-1.));
#18870=DIRECTION('',(0.,1.,0.));
#18871=DIRECTION('center_axis',(0.,-1.,0.));
#18872=DIRECTION('ref_axis',(0.,0.,-1.));
#18873=DIRECTION('center_axis',(0.,-1.,0.));
#18874=DIRECTION('ref_axis',(0.,0.,-1.));
#18875=DIRECTION('',(8.65956056235497E-17,0.707106781186545,-0.70710678118655));
#18876=DIRECTION('center_axis',(0.,1.,0.));
#18877=DIRECTION('ref_axis',(0.,0.,1.));
#18878=DIRECTION('center_axis',(0.,1.,0.));
#18879=DIRECTION('ref_axis',(1.,0.,0.));
#18880=DIRECTION('center_axis',(0.,1.,0.));
#18881=DIRECTION('ref_axis',(0.,0.,1.));
#18882=DIRECTION('',(8.65956056235496E-17,-0.707106781186545,0.70710678118655));
#18883=DIRECTION('center_axis',(0.,-1.,0.));
#18884=DIRECTION('ref_axis',(0.,0.,1.));
#18885=DIRECTION('center_axis',(0.,1.,0.));
#18886=DIRECTION('ref_axis',(0.,0.,1.));
#18887=DIRECTION('center_axis',(0.,1.,0.));
#18888=DIRECTION('ref_axis',(0.,0.,1.));
#18889=DIRECTION('',(0.,1.,0.));
#18890=DIRECTION('center_axis',(0.,1.,0.));
#18891=DIRECTION('ref_axis',(0.,0.,1.));
#18892=DIRECTION('',(8.65956056235484E-17,-0.707106781186555,0.70710678118654));
#18893=DIRECTION('center_axis',(0.,-1.,0.));
#18894=DIRECTION('ref_axis',(0.,0.,1.));
#18895=DIRECTION('center_axis',(0.,1.,0.));
#18896=DIRECTION('ref_axis',(0.,0.,1.));
#18897=DIRECTION('center_axis',(0.,1.,0.));
#18898=DIRECTION('ref_axis',(0.,0.,1.));
#18899=DIRECTION('',(0.,1.,0.));
#18900=DIRECTION('center_axis',(0.,1.,0.));
#18901=DIRECTION('ref_axis',(0.,0.,1.));
#18902=DIRECTION('',(8.65956056235496E-17,-0.707106781186545,0.70710678118655));
#18903=DIRECTION('center_axis',(0.,-1.,0.));
#18904=DIRECTION('ref_axis',(0.,0.,1.));
#18905=DIRECTION('center_axis',(0.,1.,0.));
#18906=DIRECTION('ref_axis',(0.,0.,1.));
#18907=DIRECTION('center_axis',(0.,1.,0.));
#18908=DIRECTION('ref_axis',(0.,0.,1.));
#18909=DIRECTION('',(0.,1.,0.));
#18910=DIRECTION('center_axis',(0.,-1.,0.));
#18911=DIRECTION('ref_axis',(0.,0.,1.));
#18912=DIRECTION('center_axis',(0.,-1.,0.));
#18913=DIRECTION('ref_axis',(0.,0.,1.));
#18914=DIRECTION('',(-8.65956056235496E-17,0.707106781186545,0.70710678118655));
#18915=DIRECTION('center_axis',(0.,1.,0.));
#18916=DIRECTION('ref_axis',(0.,0.,1.));
#18917=DIRECTION('center_axis',(0.,1.,0.));
#18918=DIRECTION('ref_axis',(1.,0.,0.));
#18919=DIRECTION('',(0.,0.,-1.));
#18920=DIRECTION('',(1.,0.,0.));
#18921=DIRECTION('',(0.,0.,1.));
#18922=DIRECTION('',(-1.,0.,0.));
#18923=DIRECTION('center_axis',(0.,-1.,0.));
#18924=DIRECTION('ref_axis',(0.,0.,1.));
#18925=DIRECTION('center_axis',(0.,-1.,0.));
#18926=DIRECTION('ref_axis',(0.,0.,1.));
#18927=DIRECTION('center_axis',(0.,-1.,0.));
#18928=DIRECTION('ref_axis',(0.,0.,1.));
#18929=DIRECTION('center_axis',(0.,-1.,0.));
#18930=DIRECTION('ref_axis',(0.,0.,1.));
#18931=DIRECTION('center_axis',(0.,-1.,0.));
#18932=DIRECTION('ref_axis',(1.,0.,0.));
#18933=DIRECTION('center_axis',(0.,1.,0.));
#18934=DIRECTION('ref_axis',(0.,0.,1.));
#18935=DIRECTION('',(0.,1.,0.));
#18936=DIRECTION('center_axis',(0.,-1.,0.));
#18937=DIRECTION('ref_axis',(0.,0.,1.));
#18938=DIRECTION('',(-8.65956056235484E-17,0.707106781186555,0.70710678118654));
#18939=DIRECTION('center_axis',(0.,1.,0.));
#18940=DIRECTION('ref_axis',(0.,0.,1.));
#18941=DIRECTION('center_axis',(0.,1.,0.));
#18942=DIRECTION('ref_axis',(0.,0.,1.));
#18943=DIRECTION('',(0.,1.,0.));
#18944=DIRECTION('center_axis',(0.,-1.,0.));
#18945=DIRECTION('ref_axis',(1.,4.80868578370782E-17,0.));
#18946=DIRECTION('',(0.923879532511286,0.382683432365092,1.1314261122877E-16));
#18947=DIRECTION('center_axis',(0.382683432365095,-0.923879532511285,0.));
#18948=DIRECTION('ref_axis',(0.,0.,-1.));
#18949=DIRECTION('',(-0.678598344545843,-0.281084637714823,-0.67859834454585));
#18950=DIRECTION('',(0.678598344545851,0.281084637714827,-0.678598344545841));
#18951=DIRECTION('center_axis',(0.,-0.923879532511286,0.382683432365092));
#18952=DIRECTION('ref_axis',(0.,-0.382683432365092,-0.923879532511286));
#18953=DIRECTION('',(-0.678598344545843,0.281084637714823,0.67859834454585));
#18954=DIRECTION('center_axis',(-0.382683432365095,-0.923879532511285,0.));
#18955=DIRECTION('ref_axis',(0.,0.,-1.));
#18956=DIRECTION('',(0.678598344545851,-0.281084637714827,0.678598344545841));
#18957=DIRECTION('center_axis',(0.,-0.923879532511283,-0.3826834323651));
#18958=DIRECTION('ref_axis',(0.,0.3826834323651,-0.923879532511283));
#18959=DIRECTION('center_axis',(0.,-1.,0.));
#18960=DIRECTION('ref_axis',(0.,0.,1.));
#18961=DIRECTION('',(-8.65956056235496E-17,0.707106781186545,0.70710678118655));
#18962=DIRECTION('center_axis',(0.,-1.,0.));
#18963=DIRECTION('ref_axis',(0.,0.,1.));
#18964=DIRECTION('',(-8.65956056235484E-17,0.707106781186555,0.70710678118654));
#18965=DIRECTION('center_axis',(0.,-1.,0.));
#18966=DIRECTION('ref_axis',(0.,0.,1.));
#18967=DIRECTION('',(-8.65956056235496E-17,0.707106781186545,0.70710678118655));
#18968=DIRECTION('center_axis',(-0.707106781186554,0.,-0.707106781186541));
#18969=DIRECTION('ref_axis',(-0.707106781186541,0.,0.707106781186554));
#18970=DIRECTION('center_axis',(0.707106781186554,0.,0.707106781186541));
#18971=DIRECTION('ref_axis',(0.707106781186541,0.,-0.707106781186554));
#18972=DIRECTION('center_axis',(0.707106781186548,0.,-0.707106781186548));
#18973=DIRECTION('ref_axis',(-0.707106781186548,0.,-0.707106781186548));
#18974=DIRECTION('axis',(0.,0.,1.));
#18975=DIRECTION('refdir',(1.,0.,0.));
#18976=DIRECTION('center_axis',(0.,1.,0.));
#18977=DIRECTION('ref_axis',(0.,0.,1.));
#18978=DIRECTION('center_axis',(0.,-1.,0.));
#18979=DIRECTION('ref_axis',(1.,0.,0.));
#18980=DIRECTION('center_axis',(0.,-1.,0.));
#18981=DIRECTION('ref_axis',(1.,0.,0.));
#18982=DIRECTION('center_axis',(0.,-1.,0.));
#18983=DIRECTION('ref_axis',(1.,0.,0.));
#18984=DIRECTION('',(0.707106781186548,0.707106781186547,8.65956056235494E-17));
#18985=DIRECTION('center_axis',(0.,-1.,0.));
#18986=DIRECTION('ref_axis',(1.,0.,0.));
#18987=DIRECTION('center_axis',(0.,-1.,0.));
#18988=DIRECTION('ref_axis',(1.,0.,0.));
#18989=DIRECTION('',(0.,1.,0.));
#18990=DIRECTION('center_axis',(0.,1.,0.));
#18991=DIRECTION('ref_axis',(1.,0.,0.));
#18992=DIRECTION('center_axis',(0.,-1.,0.));
#18993=DIRECTION('ref_axis',(1.,0.,0.));
#18994=DIRECTION('',(-0.707106781186549,0.707106781186546,-8.65956056235495E-17));
#18995=DIRECTION('center_axis',(0.,-1.,0.));
#18996=DIRECTION('ref_axis',(0.,0.,-1.));
#18997=DIRECTION('axis',(0.,0.,1.));
#18998=DIRECTION('refdir',(1.,0.,0.));
#18999=DIRECTION('center_axis',(0.,-1.,0.));
#19000=DIRECTION('ref_axis',(1.,0.,0.));
#19001=DIRECTION('',(0.,1.,0.));
#19002=DIRECTION('',(0.,-1.,0.));
#19003=DIRECTION('center_axis',(0.,-1.,0.));
#19004=DIRECTION('ref_axis',(1.,0.,0.));
#19005=DIRECTION('',(0.,1.,0.));
#19006=DIRECTION('center_axis',(0.,-1.,0.));
#19007=DIRECTION('ref_axis',(0.738759972569494,1.07840993164173E-17,-0.673968621620562));
#19008=DIRECTION('',(0.,-1.,0.));
#19009=DIRECTION('center_axis',(0.,-1.,0.));
#19010=DIRECTION('ref_axis',(1.,1.07840993164173E-17,0.));
#19011=DIRECTION('center_axis',(0.,-1.,0.));
#19012=DIRECTION('ref_axis',(1.,1.07840993164173E-17,0.));
#19013=DIRECTION('',(0.,-1.,0.));
#19014=DIRECTION('center_axis',(0.,1.,0.));
#19015=DIRECTION('ref_axis',(1.,1.07840993164173E-17,0.));
#19016=DIRECTION('center_axis',(0.,1.,0.));
#19017=DIRECTION('ref_axis',(0.,0.,1.));
#19018=DIRECTION('',(-1.,0.,0.));
#19019=DIRECTION('center_axis',(0.,-1.,0.));
#19020=DIRECTION('ref_axis',(1.,0.,0.));
#19021=DIRECTION('center_axis',(0.,1.,0.));
#19022=DIRECTION('ref_axis',(0.,0.,1.));
#19023=DIRECTION('',(1.,0.,0.));
#19024=DIRECTION('center_axis',(0.,-1.,0.));
#19025=DIRECTION('ref_axis',(1.,0.,0.));
#19026=DIRECTION('',(1.,0.,0.));
#19027=DIRECTION('center_axis',(0.,1.,0.));
#19028=DIRECTION('ref_axis',(1.,1.07840993164173E-17,0.));
#19029=DIRECTION('center_axis',(0.,1.,0.));
#19030=DIRECTION('ref_axis',(0.,0.,1.));
#19031=DIRECTION('',(-1.,0.,0.));
#19032=DIRECTION('center_axis',(0.,-1.,0.));
#19033=DIRECTION('ref_axis',(1.,0.,0.));
#19034=DIRECTION('center_axis',(0.,-1.,0.));
#19035=DIRECTION('ref_axis',(1.,1.07840993164173E-17,0.));
#19036=DIRECTION('',(0.,-1.,0.));
#19037=DIRECTION('',(0.,1.,0.));
#19038=DIRECTION('center_axis',(0.,1.,0.));
#19039=DIRECTION('ref_axis',(1.,1.07840993164173E-17,0.));
#19040=DIRECTION('center_axis',(0.,-1.,0.));
#19041=DIRECTION('ref_axis',(1.,1.07840993164173E-17,0.));
#19042=DIRECTION('',(0.,1.,0.));
#19043=DIRECTION('center_axis',(0.,1.,0.));
#19044=DIRECTION('ref_axis',(0.,0.,1.));
#19045=DIRECTION('center_axis',(0.,1.,0.));
#19046=DIRECTION('ref_axis',(1.,0.,0.));
#19047=DIRECTION('center_axis',(0.,1.,0.));
#19048=DIRECTION('ref_axis',(1.,0.,0.));
#19049=DIRECTION('center_axis',(0.,0.,-1.));
#19050=DIRECTION('ref_axis',(1.,0.,0.));
#19051=DIRECTION('',(1.,0.,0.));
#19052=DIRECTION('',(0.,1.,0.));
#19053=DIRECTION('',(1.,0.,0.));
#19054=DIRECTION('center_axis',(0.,0.,-1.));
#19055=DIRECTION('ref_axis',(1.,0.,0.));
#19056=DIRECTION('',(1.,0.,0.));
#19057=DIRECTION('',(0.,-1.,0.));
#19058=DIRECTION('',(1.,0.,0.));
#19059=DIRECTION('center_axis',(0.,-1.,0.));
#19060=DIRECTION('ref_axis',(-0.736568605701436,0.,-0.676362838345694));
#19061=DIRECTION('center_axis',(0.,1.,0.));
#19062=DIRECTION('ref_axis',(1.,0.,0.));
#19063=DIRECTION('center_axis',(0.,-1.,0.));
#19064=DIRECTION('ref_axis',(1.,0.,0.));
#19065=DIRECTION('',(0.,1.,0.));
#19066=DIRECTION('center_axis',(0.,-1.,0.));
#19067=DIRECTION('ref_axis',(1.,0.,0.));
#19068=DIRECTION('center_axis',(0.,-1.,0.));
#19069=DIRECTION('ref_axis',(0.,0.,-1.));
#19070=DIRECTION('',(-1.,0.,0.));
#19071=DIRECTION('center_axis',(0.,1.,0.));
#19072=DIRECTION('ref_axis',(1.,0.,0.));
#19073=DIRECTION('center_axis',(0.,1.,0.));
#19074=DIRECTION('ref_axis',(1.,0.,0.));
#19075=DIRECTION('center_axis',(0.,0.,1.));
#19076=DIRECTION('ref_axis',(-1.,0.,0.));
#19077=DIRECTION('',(-1.,0.,0.));
#19078=DIRECTION('',(0.,1.,0.));
#19079=DIRECTION('center_axis',(0.,-1.,0.));
#19080=DIRECTION('ref_axis',(0.,0.,-1.));
#19081=DIRECTION('center_axis',(0.,1.,0.));
#19082=DIRECTION('ref_axis',(1.,0.,0.));
#19083=DIRECTION('',(-1.,0.,0.));
#19084=DIRECTION('center_axis',(0.,0.,1.));
#19085=DIRECTION('ref_axis',(-1.,0.,0.));
#19086=DIRECTION('',(0.,-1.,0.));
#19087=DIRECTION('',(-1.,0.,0.));
#19088=DIRECTION('center_axis',(0.,-1.,0.));
#19089=DIRECTION('ref_axis',(1.,0.,0.));
#19090=DIRECTION('center_axis',(0.,-1.,0.));
#19091=DIRECTION('ref_axis',(1.,0.,0.));
#19092=DIRECTION('',(0.,1.,0.));
#19093=DIRECTION('center_axis',(0.,-1.,0.));
#19094=DIRECTION('ref_axis',(1.,0.,0.));
#19095=DIRECTION('center_axis',(0.,-1.,0.));
#19096=DIRECTION('ref_axis',(1.,0.,0.));
#19097=DIRECTION('center_axis',(0.,-1.,0.));
#19098=DIRECTION('ref_axis',(1.,0.,0.));
#19099=DIRECTION('center_axis',(0.,-1.,0.));
#19100=DIRECTION('ref_axis',(1.,0.,0.));
#19101=DIRECTION('center_axis',(0.,-1.,0.));
#19102=DIRECTION('ref_axis',(1.,0.,0.));
#19103=DIRECTION('center_axis',(0.,-1.,0.));
#19104=DIRECTION('ref_axis',(1.,0.,0.));
#19105=DIRECTION('center_axis',(0.,1.,0.));
#19106=DIRECTION('ref_axis',(0.,0.,1.));
#19107=DIRECTION('center_axis',(0.,-1.,0.));
#19108=DIRECTION('ref_axis',(1.,0.,0.));
#19109=DIRECTION('center_axis',(0.,1.,0.));
#19110=DIRECTION('ref_axis',(0.,0.,1.));
#19111=DIRECTION('center_axis',(0.,-1.,0.));
#19112=DIRECTION('ref_axis',(1.,0.,0.));
#19113=DIRECTION('center_axis',(0.,1.,0.));
#19114=DIRECTION('ref_axis',(1.,0.,0.));
#19115=DIRECTION('center_axis',(0.,1.,0.));
#19116=DIRECTION('ref_axis',(1.,0.,0.));
#19117=DIRECTION('center_axis',(0.,1.,0.));
#19118=DIRECTION('ref_axis',(1.,0.,0.));
#19119=DIRECTION('center_axis',(0.,-1.,0.));
#19120=DIRECTION('ref_axis',(1.,0.,0.));
#19121=DIRECTION('',(-0.707106781186548,0.707106781186548,-8.65956056235493E-17));
#19122=DIRECTION('center_axis',(0.,-1.,0.));
#19123=DIRECTION('ref_axis',(0.,0.,-1.));
#19124=DIRECTION('axis',(0.,0.,1.));
#19125=DIRECTION('refdir',(1.,0.,0.));
#19126=DIRECTION('center_axis',(0.,0.,1.));
#19127=DIRECTION('ref_axis',(1.,0.,0.));
#19128=DIRECTION('',(0.,0.,-1.));
#19129=DIRECTION('center_axis',(0.,0.,1.));
#19130=DIRECTION('ref_axis',(1.,0.,0.));
#19131=DIRECTION('center_axis',(0.,0.,1.));
#19132=DIRECTION('ref_axis',(1.,0.,0.));
#19133=DIRECTION('',(0.,0.,-1.));
#19134=DIRECTION('center_axis',(0.,0.,1.));
#19135=DIRECTION('ref_axis',(1.,0.,0.));
#19136=DIRECTION('',(0.,0.,-1.));
#19137=DIRECTION('center_axis',(0.,0.,1.));
#19138=DIRECTION('ref_axis',(1.,0.,0.));
#19139=DIRECTION('',(0.,0.,-1.));
#19140=DIRECTION('center_axis',(0.,0.,1.));
#19141=DIRECTION('ref_axis',(1.,0.,0.));
#19142=DIRECTION('',(0.,0.,-1.));
#19143=DIRECTION('center_axis',(0.,0.,1.));
#19144=DIRECTION('ref_axis',(1.,0.,0.));
#19145=DIRECTION('',(0.,0.,-1.));
#19146=DIRECTION('center_axis',(0.,0.,1.));
#19147=DIRECTION('ref_axis',(-0.131102582345095,-0.991368807711059,0.));
#19148=DIRECTION('',(0.,0.,1.));
#19149=DIRECTION('center_axis',(0.,0.,1.));
#19150=DIRECTION('ref_axis',(1.,1.81591784523378E-14,0.));
#19151=DIRECTION('center_axis',(0.,0.,1.));
#19152=DIRECTION('ref_axis',(1.,1.81591784523378E-14,0.));
#19153=DIRECTION('',(0.,0.,1.));
#19154=DIRECTION('center_axis',(0.,0.,1.));
#19155=DIRECTION('ref_axis',(1.,1.81591784523378E-14,0.));
#19156=DIRECTION('',(0.,0.,1.));
#19157=DIRECTION('center_axis',(0.,0.,1.));
#19158=DIRECTION('ref_axis',(1.,1.81591784523378E-14,0.));
#19159=DIRECTION('',(0.,0.,1.));
#19160=DIRECTION('center_axis',(0.,0.,1.));
#19161=DIRECTION('ref_axis',(1.,1.81591784523378E-14,0.));
#19162=DIRECTION('',(0.,0.,1.));
#19163=DIRECTION('center_axis',(0.,0.,1.));
#19164=DIRECTION('ref_axis',(1.,1.81591784523378E-14,0.));
#19165=DIRECTION('',(0.,0.,1.));
#19166=DIRECTION('center_axis',(0.,0.,1.));
#19167=DIRECTION('ref_axis',(1.,0.,0.));
#19168=DIRECTION('center_axis',(0.,0.,-1.));
#19169=DIRECTION('ref_axis',(1.,0.,0.));
#19170=DIRECTION('center_axis',(0.,0.,-1.));
#19171=DIRECTION('ref_axis',(1.,0.,0.));
#19172=DIRECTION('center_axis',(0.,0.,1.));
#19173=DIRECTION('ref_axis',(1.,0.,0.));
#19174=DIRECTION('center_axis',(0.,0.,1.));
#19175=DIRECTION('ref_axis',(1.,0.,0.));
#19176=DIRECTION('center_axis',(0.,0.,1.));
#19177=DIRECTION('ref_axis',(1.,0.,0.));
#19178=DIRECTION('center_axis',(0.,0.,-1.));
#19179=DIRECTION('ref_axis',(1.,1.81591784523378E-14,0.));
#19180=DIRECTION('center_axis',(0.,0.,1.));
#19181=DIRECTION('ref_axis',(1.,1.81591784523378E-14,0.));
#19182=DIRECTION('center_axis',(0.,0.,1.));
#19183=DIRECTION('ref_axis',(1.,0.,0.));
#19184=DIRECTION('',(-1.,2.40370335797945E-16,0.));
#19185=DIRECTION('center_axis',(0.,0.,1.));
#19186=DIRECTION('ref_axis',(1.,0.,0.));
#19187=DIRECTION('center_axis',(0.,0.,1.));
#19188=DIRECTION('ref_axis',(1.,0.,0.));
#19189=DIRECTION('',(-0.5,0.866025403784439,0.));
#19190=DIRECTION('center_axis',(0.,0.,1.));
#19191=DIRECTION('ref_axis',(1.,0.,0.));
#19192=DIRECTION('center_axis',(0.,0.,1.));
#19193=DIRECTION('ref_axis',(1.,0.,0.));
#19194=DIRECTION('',(0.5,0.866025403784439,0.));
#19195=DIRECTION('center_axis',(0.,0.,1.));
#19196=DIRECTION('ref_axis',(1.,0.,0.));
#19197=DIRECTION('center_axis',(0.,0.,1.));
#19198=DIRECTION('ref_axis',(1.,0.,0.));
#19199=DIRECTION('',(1.,-1.20185167898973E-16,0.));
#19200=DIRECTION('center_axis',(0.,0.,1.));
#19201=DIRECTION('ref_axis',(1.,0.,0.));
#19202=DIRECTION('center_axis',(0.,0.,1.));
#19203=DIRECTION('ref_axis',(1.,0.,0.));
#19204=DIRECTION('',(0.5,-0.866025403784439,0.));
#19205=DIRECTION('center_axis',(0.,0.,1.));
#19206=DIRECTION('ref_axis',(1.,0.,0.));
#19207=DIRECTION('center_axis',(0.,0.,1.));
#19208=DIRECTION('ref_axis',(1.,0.,0.));
#19209=DIRECTION('',(-0.5,-0.866025403784439,0.));
#19210=DIRECTION('center_axis',(0.,0.,1.));
#19211=DIRECTION('ref_axis',(1.,0.,0.));
#19212=DIRECTION('center_axis',(0.,0.,1.));
#19213=DIRECTION('ref_axis',(1.,0.,0.));
#19214=DIRECTION('',(-0.854211984955561,-1.04610797316913E-16,0.519924883765223));
#19215=DIRECTION('center_axis',(0.,0.,-1.));
#19216=DIRECTION('ref_axis',(1.,0.,0.));
#19217=DIRECTION('center_axis',(0.,0.,-1.));
#19218=DIRECTION('ref_axis',(1.,0.,0.));
#19219=DIRECTION('center_axis',(0.,0.,-1.));
#19220=DIRECTION('ref_axis',(1.,0.,0.));
#19221=DIRECTION('center_axis',(0.,0.,-1.));
#19222=DIRECTION('ref_axis',(1.,0.,0.));
#19223=DIRECTION('center_axis',(0.,0.,-1.));
#19224=DIRECTION('ref_axis',(1.,0.,0.));
#19225=DIRECTION('center_axis',(0.,0.,-1.));
#19226=DIRECTION('ref_axis',(1.,0.,0.));
#19227=DIRECTION('center_axis',(0.,0.,-1.));
#19228=DIRECTION('ref_axis',(1.,0.,0.));
#19229=DIRECTION('center_axis',(-0.866025403784439,0.5,0.));
#19230=DIRECTION('ref_axis',(0.5,0.866025403784439,0.));
#19231=DIRECTION('',(0.,0.,-1.));
#19232=DIRECTION('',(0.5,0.866025403784439,0.));
#19233=DIRECTION('',(0.,0.,-1.));
#19234=DIRECTION('center_axis',(-0.866025403784439,0.5,0.));
#19235=DIRECTION('ref_axis',(0.5,0.866025403784439,0.));
#19236=DIRECTION('',(0.,0.,-1.));
#19237=DIRECTION('',(0.5,0.866025403784439,0.));
#19238=DIRECTION('center_axis',(1.20185167898973E-16,1.,0.));
#19239=DIRECTION('ref_axis',(1.,-1.20185167898973E-16,0.));
#19240=DIRECTION('',(0.,0.,-1.));
#19241=DIRECTION('',(1.,-1.20185167898973E-16,0.));
#19242=DIRECTION('center_axis',(1.20185167898973E-16,1.,0.));
#19243=DIRECTION('ref_axis',(1.,-1.20185167898973E-16,0.));
#19244=DIRECTION('',(1.,-1.20185167898973E-16,0.));
#19245=DIRECTION('',(0.,0.,-1.));
#19246=DIRECTION('center_axis',(1.20185167898973E-16,1.,0.));
#19247=DIRECTION('ref_axis',(1.,-1.20185167898973E-16,0.));
#19248=DIRECTION('',(0.,0.,-1.));
#19249=DIRECTION('',(1.,-1.20185167898973E-16,0.));
#19250=DIRECTION('center_axis',(-0.866025403784439,-0.5,0.));
#19251=DIRECTION('ref_axis',(-0.5,0.866025403784439,0.));
#19252=DIRECTION('',(-0.5,0.866025403784439,0.));
#19253=DIRECTION('',(0.,0.,-1.));
#19254=DIRECTION('center_axis',(-0.866025403784439,-0.5,0.));
#19255=DIRECTION('ref_axis',(-0.5,0.866025403784439,0.));
#19256=DIRECTION('',(0.,0.,-1.));
#19257=DIRECTION('',(-0.5,0.866025403784439,0.));
#19258=DIRECTION('center_axis',(0.866025403784439,0.5,0.));
#19259=DIRECTION('ref_axis',(0.5,-0.866025403784439,0.));
#19260=DIRECTION('',(0.,0.,-1.));
#19261=DIRECTION('',(0.5,-0.866025403784439,0.));
#19262=DIRECTION('center_axis',(0.866025403784439,0.5,0.));
#19263=DIRECTION('ref_axis',(0.5,-0.866025403784439,0.));
#19264=DIRECTION('',(0.5,-0.866025403784439,0.));
#19265=DIRECTION('',(0.,0.,-1.));
#19266=DIRECTION('center_axis',(0.866025403784439,0.5,0.));
#19267=DIRECTION('ref_axis',(0.5,-0.866025403784439,0.));
#19268=DIRECTION('',(0.5,-0.866025403784439,0.));
#19269=DIRECTION('center_axis',(0.,0.,-1.));
#19270=DIRECTION('ref_axis',(-1.,0.,0.));
#19271=DIRECTION('',(0.5,0.866025403784439,0.));
#19272=DIRECTION('center_axis',(0.,0.,-1.));
#19273=DIRECTION('ref_axis',(-1.,0.,0.));
#19274=DIRECTION('center_axis',(0.,0.,-1.));
#19275=DIRECTION('ref_axis',(-1.,0.,0.));
#19276=DIRECTION('',(-0.5,-0.866025403784439,0.));
#19277=DIRECTION('center_axis',(0.,0.,-1.));
#19278=DIRECTION('ref_axis',(-1.,0.,0.));
#19279=DIRECTION('',(-1.,2.40370335797945E-16,0.));
#19280=DIRECTION('',(-0.5,-0.866025403784439,0.));
#19281=DIRECTION('center_axis',(0.,0.,-1.));
#19282=DIRECTION('ref_axis',(-1.,0.,0.));
#19283=DIRECTION('',(-1.,2.40370335797945E-16,0.));
#19284=DIRECTION('center_axis',(0.,0.,-1.));
#19285=DIRECTION('ref_axis',(-1.,0.,0.));
#19286=DIRECTION('',(-0.5,0.866025403784439,0.));
#19287=DIRECTION('center_axis',(0.866025403784439,-0.5,0.));
#19288=DIRECTION('ref_axis',(-0.5,-0.866025403784439,0.));
#19289=DIRECTION('',(0.,0.,-1.));
#19290=DIRECTION('',(-0.5,-0.866025403784439,0.));
#19291=DIRECTION('center_axis',(0.866025403784439,-0.5,0.));
#19292=DIRECTION('ref_axis',(-0.5,-0.866025403784439,0.));
#19293=DIRECTION('',(0.,0.,-1.));
#19294=DIRECTION('center_axis',(0.866025403784439,-0.5,0.));
#19295=DIRECTION('ref_axis',(-0.5,-0.866025403784439,0.));
#19296=DIRECTION('center_axis',(-2.40370335797945E-16,-1.,0.));
#19297=DIRECTION('ref_axis',(-1.,2.40370335797945E-16,0.));
#19298=DIRECTION('center_axis',(-2.40370335797945E-16,-1.,0.));
#19299=DIRECTION('ref_axis',(-1.,2.40370335797945E-16,0.));
#19300=DIRECTION('',(-1.,2.40370335797945E-16,0.));
#19301=DIRECTION('center_axis',(-0.866025403784439,0.5,0.));
#19302=DIRECTION('ref_axis',(0.5,0.866025403784439,0.));
#19303=DIRECTION('center_axis',(-0.866025403784439,-0.5,0.));
#19304=DIRECTION('ref_axis',(-0.5,0.866025403784439,0.));
#19305=DIRECTION('center_axis',(-2.40370335797945E-16,-1.,0.));
#19306=DIRECTION('ref_axis',(-1.,2.40370335797945E-16,0.));
#19307=DIRECTION('center_axis',(0.,0.,-1.));
#19308=DIRECTION('ref_axis',(-1.,0.,0.));
#19309=DIRECTION('center_axis',(0.,0.,1.));
#19310=DIRECTION('ref_axis',(1.,0.,0.));
#19311=DIRECTION('center_axis',(0.,0.,1.));
#19312=DIRECTION('ref_axis',(1.,0.,0.));
#19313=DIRECTION('',(0.832050294337844,1.01896772969045E-16,-0.554700196225229));
#19314=DIRECTION('center_axis',(0.,0.,1.));
#19315=DIRECTION('ref_axis',(1.,0.,0.));
#19316=DIRECTION('center_axis',(0.,0.,-1.));
#19317=DIRECTION('ref_axis',(1.,0.,0.));
#19318=DIRECTION('center_axis',(0.,0.,-1.));
#19319=DIRECTION('ref_axis',(1.,0.,0.));
#19320=DIRECTION('center_axis',(0.,0.,1.));
#19321=DIRECTION('ref_axis',(1.,0.,0.));
#19322=DIRECTION('',(-0.707106781186548,-8.65956056235494E-17,-0.707106781186547));
#19323=DIRECTION('center_axis',(0.,0.,1.));
#19324=DIRECTION('ref_axis',(1.,0.,0.));
#19325=DIRECTION('axis',(0.,0.,1.));
#19326=DIRECTION('refdir',(1.,0.,0.));
#19327=DIRECTION('center_axis',(0.,0.,1.));
#19328=DIRECTION('ref_axis',(1.,0.,0.));
#19329=DIRECTION('',(0.,0.,-1.));
#19330=DIRECTION('center_axis',(0.,0.,1.));
#19331=DIRECTION('ref_axis',(1.,0.,0.));
#19332=DIRECTION('center_axis',(0.,0.,1.));
#19333=DIRECTION('ref_axis',(1.,0.,0.));
#19334=DIRECTION('',(0.,0.,-1.));
#19335=DIRECTION('center_axis',(0.,0.,1.));
#19336=DIRECTION('ref_axis',(1.,0.,0.));
#19337=DIRECTION('',(0.,0.,-1.));
#19338=DIRECTION('center_axis',(0.,0.,1.));
#19339=DIRECTION('ref_axis',(1.,0.,0.));
#19340=DIRECTION('',(0.,0.,-1.));
#19341=DIRECTION('center_axis',(0.,0.,1.));
#19342=DIRECTION('ref_axis',(1.,0.,0.));
#19343=DIRECTION('',(0.,0.,-1.));
#19344=DIRECTION('center_axis',(0.,0.,1.));
#19345=DIRECTION('ref_axis',(1.,3.07677254327731E-16,0.));
#19346=DIRECTION('',(0.,0.,1.));
#19347=DIRECTION('center_axis',(0.,0.,1.));
#19348=DIRECTION('ref_axis',(1.,3.07677254327731E-16,0.));
#19349=DIRECTION('center_axis',(0.,0.,1.));
#19350=DIRECTION('ref_axis',(1.,3.07677254327731E-16,0.));
#19351=DIRECTION('',(0.,0.,1.));
#19352=DIRECTION('center_axis',(0.,0.,1.));
#19353=DIRECTION('ref_axis',(1.,3.07677254327731E-16,0.));
#19354=DIRECTION('center_axis',(0.,0.,1.));
#19355=DIRECTION('ref_axis',(1.,3.07677254327731E-16,0.));
#19356=DIRECTION('',(0.,0.,1.));
#19357=DIRECTION('center_axis',(0.,0.,1.));
#19358=DIRECTION('ref_axis',(1.,3.07677254327731E-16,0.));
#19359=DIRECTION('',(0.,0.,1.));
#19360=DIRECTION('center_axis',(0.,0.,1.));
#19361=DIRECTION('ref_axis',(1.,3.07677254327731E-16,0.));
#19362=DIRECTION('',(0.,0.,1.));
#19363=DIRECTION('center_axis',(0.,0.,1.));
#19364=DIRECTION('ref_axis',(1.,0.,0.));
#19365=DIRECTION('center_axis',(0.,0.,-1.));
#19366=DIRECTION('ref_axis',(1.,0.,0.));
#19367=DIRECTION('center_axis',(0.,0.,-1.));
#19368=DIRECTION('ref_axis',(1.,0.,0.));
#19369=DIRECTION('center_axis',(0.,0.,1.));
#19370=DIRECTION('ref_axis',(1.,0.,0.));
#19371=DIRECTION('center_axis',(0.,0.,1.));
#19372=DIRECTION('ref_axis',(1.,0.,0.));
#19373=DIRECTION('center_axis',(0.,0.,1.));
#19374=DIRECTION('ref_axis',(1.,0.,0.));
#19375=DIRECTION('center_axis',(0.,0.,-1.));
#19376=DIRECTION('ref_axis',(1.,3.07677254327731E-16,0.));
#19377=DIRECTION('center_axis',(0.,0.,1.));
#19378=DIRECTION('ref_axis',(0.889158769900871,0.457598822013749,0.));
#19379=DIRECTION('center_axis',(0.,0.,1.));
#19380=DIRECTION('ref_axis',(1.,0.,0.));
#19381=DIRECTION('',(-1.,2.40370335797945E-16,0.));
#19382=DIRECTION('center_axis',(0.,0.,1.));
#19383=DIRECTION('ref_axis',(1.,0.,0.));
#19384=DIRECTION('center_axis',(0.,0.,1.));
#19385=DIRECTION('ref_axis',(1.,0.,0.));
#19386=DIRECTION('',(-0.5,0.866025403784439,0.));
#19387=DIRECTION('center_axis',(0.,0.,1.));
#19388=DIRECTION('ref_axis',(1.,0.,0.));
#19389=DIRECTION('center_axis',(0.,0.,1.));
#19390=DIRECTION('ref_axis',(1.,0.,0.));
#19391=DIRECTION('',(0.5,0.866025403784439,0.));
#19392=DIRECTION('center_axis',(0.,0.,1.));
#19393=DIRECTION('ref_axis',(1.,0.,0.));
#19394=DIRECTION('center_axis',(0.,0.,1.));
#19395=DIRECTION('ref_axis',(1.,0.,0.));
#19396=DIRECTION('',(1.,-1.20185167898973E-16,0.));
#19397=DIRECTION('center_axis',(0.,0.,1.));
#19398=DIRECTION('ref_axis',(1.,0.,0.));
#19399=DIRECTION('center_axis',(0.,0.,1.));
#19400=DIRECTION('ref_axis',(1.,0.,0.));
#19401=DIRECTION('',(0.5,-0.866025403784439,0.));
#19402=DIRECTION('center_axis',(0.,0.,1.));
#19403=DIRECTION('ref_axis',(1.,0.,0.));
#19404=DIRECTION('center_axis',(0.,0.,1.));
#19405=DIRECTION('ref_axis',(1.,0.,0.));
#19406=DIRECTION('',(-0.5,-0.866025403784439,0.));
#19407=DIRECTION('center_axis',(0.,0.,1.));
#19408=DIRECTION('ref_axis',(1.,0.,0.));
#19409=DIRECTION('center_axis',(0.,0.,1.));
#19410=DIRECTION('ref_axis',(1.,0.,0.));
#19411=DIRECTION('',(-0.854211984955561,-1.04610797316913E-16,0.519924883765223));
#19412=DIRECTION('center_axis',(0.,0.,-1.));
#19413=DIRECTION('ref_axis',(1.,0.,0.));
#19414=DIRECTION('center_axis',(0.,0.,-1.));
#19415=DIRECTION('ref_axis',(1.,0.,0.));
#19416=DIRECTION('center_axis',(0.,0.,-1.));
#19417=DIRECTION('ref_axis',(1.,0.,0.));
#19418=DIRECTION('center_axis',(0.,0.,-1.));
#19419=DIRECTION('ref_axis',(1.,0.,0.));
#19420=DIRECTION('center_axis',(0.,0.,-1.));
#19421=DIRECTION('ref_axis',(1.,0.,0.));
#19422=DIRECTION('center_axis',(0.,0.,-1.));
#19423=DIRECTION('ref_axis',(1.,0.,0.));
#19424=DIRECTION('center_axis',(0.,0.,-1.));
#19425=DIRECTION('ref_axis',(1.,0.,0.));
#19426=DIRECTION('center_axis',(-0.866025403784439,0.5,0.));
#19427=DIRECTION('ref_axis',(0.5,0.866025403784439,0.));
#19428=DIRECTION('',(0.,0.,-1.));
#19429=DIRECTION('',(0.5,0.866025403784439,0.));
#19430=DIRECTION('',(0.,0.,-1.));
#19431=DIRECTION('center_axis',(-0.866025403784439,0.5,0.));
#19432=DIRECTION('ref_axis',(0.5,0.866025403784439,0.));
#19433=DIRECTION('',(0.,0.,-1.));
#19434=DIRECTION('',(0.5,0.866025403784439,0.));
#19435=DIRECTION('center_axis',(1.20185167898973E-16,1.,0.));
#19436=DIRECTION('ref_axis',(1.,-1.20185167898973E-16,0.));
#19437=DIRECTION('',(0.,0.,-1.));
#19438=DIRECTION('',(1.,-1.20185167898973E-16,0.));
#19439=DIRECTION('center_axis',(1.20185167898973E-16,1.,0.));
#19440=DIRECTION('ref_axis',(1.,-1.20185167898973E-16,0.));
#19441=DIRECTION('',(1.,-1.20185167898973E-16,0.));
#19442=DIRECTION('',(0.,0.,-1.));
#19443=DIRECTION('center_axis',(1.20185167898973E-16,1.,0.));
#19444=DIRECTION('ref_axis',(1.,-1.20185167898973E-16,0.));
#19445=DIRECTION('',(0.,0.,-1.));
#19446=DIRECTION('',(1.,-1.20185167898973E-16,0.));
#19447=DIRECTION('center_axis',(-0.866025403784439,-0.5,0.));
#19448=DIRECTION('ref_axis',(-0.5,0.866025403784439,0.));
#19449=DIRECTION('',(-0.5,0.866025403784439,0.));
#19450=DIRECTION('',(0.,0.,-1.));
#19451=DIRECTION('center_axis',(-0.866025403784439,-0.5,0.));
#19452=DIRECTION('ref_axis',(-0.5,0.866025403784439,0.));
#19453=DIRECTION('',(0.,0.,-1.));
#19454=DIRECTION('',(-0.5,0.866025403784439,0.));
#19455=DIRECTION('center_axis',(0.866025403784439,0.5,0.));
#19456=DIRECTION('ref_axis',(0.5,-0.866025403784439,0.));
#19457=DIRECTION('',(0.,0.,-1.));
#19458=DIRECTION('',(0.5,-0.866025403784439,0.));
#19459=DIRECTION('center_axis',(0.866025403784439,0.5,0.));
#19460=DIRECTION('ref_axis',(0.5,-0.866025403784439,0.));
#19461=DIRECTION('',(0.5,-0.866025403784439,0.));
#19462=DIRECTION('',(0.,0.,-1.));
#19463=DIRECTION('center_axis',(0.866025403784439,0.5,0.));
#19464=DIRECTION('ref_axis',(0.5,-0.866025403784439,0.));
#19465=DIRECTION('',(0.5,-0.866025403784439,0.));
#19466=DIRECTION('center_axis',(0.,0.,-1.));
#19467=DIRECTION('ref_axis',(-1.,0.,0.));
#19468=DIRECTION('',(0.5,0.866025403784439,0.));
#19469=DIRECTION('center_axis',(0.,0.,-1.));
#19470=DIRECTION('ref_axis',(-1.,0.,0.));
#19471=DIRECTION('center_axis',(0.,0.,-1.));
#19472=DIRECTION('ref_axis',(-1.,0.,0.));
#19473=DIRECTION('',(-0.5,-0.866025403784439,0.));
#19474=DIRECTION('center_axis',(0.,0.,-1.));
#19475=DIRECTION('ref_axis',(-1.,0.,0.));
#19476=DIRECTION('',(-1.,2.40370335797945E-16,0.));
#19477=DIRECTION('',(-0.5,-0.866025403784439,0.));
#19478=DIRECTION('center_axis',(0.,0.,-1.));
#19479=DIRECTION('ref_axis',(-1.,0.,0.));
#19480=DIRECTION('',(-1.,2.40370335797945E-16,0.));
#19481=DIRECTION('center_axis',(0.,0.,-1.));
#19482=DIRECTION('ref_axis',(-1.,0.,0.));
#19483=DIRECTION('',(-0.5,0.866025403784439,0.));
#19484=DIRECTION('center_axis',(0.866025403784439,-0.5,0.));
#19485=DIRECTION('ref_axis',(-0.5,-0.866025403784439,0.));
#19486=DIRECTION('',(0.,0.,-1.));
#19487=DIRECTION('',(-0.5,-0.866025403784439,0.));
#19488=DIRECTION('center_axis',(0.866025403784439,-0.5,0.));
#19489=DIRECTION('ref_axis',(-0.5,-0.866025403784439,0.));
#19490=DIRECTION('',(0.,0.,-1.));
#19491=DIRECTION('center_axis',(0.866025403784439,-0.5,0.));
#19492=DIRECTION('ref_axis',(-0.5,-0.866025403784439,0.));
#19493=DIRECTION('center_axis',(-2.40370335797945E-16,-1.,0.));
#19494=DIRECTION('ref_axis',(-1.,2.40370335797945E-16,0.));
#19495=DIRECTION('center_axis',(-2.40370335797945E-16,-1.,0.));
#19496=DIRECTION('ref_axis',(-1.,2.40370335797945E-16,0.));
#19497=DIRECTION('',(-1.,2.40370335797945E-16,0.));
#19498=DIRECTION('center_axis',(-0.866025403784439,0.5,0.));
#19499=DIRECTION('ref_axis',(0.5,0.866025403784439,0.));
#19500=DIRECTION('center_axis',(-0.866025403784439,-0.5,0.));
#19501=DIRECTION('ref_axis',(-0.5,0.866025403784439,0.));
#19502=DIRECTION('center_axis',(-2.40370335797945E-16,-1.,0.));
#19503=DIRECTION('ref_axis',(-1.,2.40370335797945E-16,0.));
#19504=DIRECTION('center_axis',(0.,0.,-1.));
#19505=DIRECTION('ref_axis',(-1.,0.,0.));
#19506=DIRECTION('center_axis',(0.,0.,1.));
#19507=DIRECTION('ref_axis',(1.,0.,0.));
#19508=DIRECTION('center_axis',(0.,0.,1.));
#19509=DIRECTION('ref_axis',(1.,0.,0.));
#19510=DIRECTION('',(0.832050294337843,1.01896772969045E-16,-0.554700196225229));
#19511=DIRECTION('center_axis',(0.,0.,1.));
#19512=DIRECTION('ref_axis',(1.,0.,0.));
#19513=DIRECTION('center_axis',(0.,0.,-1.));
#19514=DIRECTION('ref_axis',(1.,0.,0.));
#19515=DIRECTION('center_axis',(0.,0.,-1.));
#19516=DIRECTION('ref_axis',(1.,0.,0.));
#19517=DIRECTION('center_axis',(0.,0.,1.));
#19518=DIRECTION('ref_axis',(1.,0.,0.));
#19519=DIRECTION('',(-0.707106781186548,-8.65956056235494E-17,-0.707106781186547));
#19520=DIRECTION('center_axis',(0.,0.,1.));
#19521=DIRECTION('ref_axis',(1.,0.,0.));
#19522=DIRECTION('axis',(0.,0.,1.));
#19523=DIRECTION('refdir',(1.,0.,0.));
#19524=DIRECTION('center_axis',(0.,-0.38268343236508,0.923879532511291));
#19525=DIRECTION('ref_axis',(1.,0.,0.));
#19526=DIRECTION('',(0.357406744336593,-0.86285620946102,-0.357406744336584));
#19527=DIRECTION('',(1.,0.,0.));
#19528=DIRECTION('',(0.357406744336593,0.86285620946102,0.357406744336584));
#19529=DIRECTION('',(-0.357406744336581,0.862856209461025,0.357406744336586));
#19530=DIRECTION('',(-1.,0.,0.));
#19531=DIRECTION('',(-0.357406744336581,-0.862856209461025,-0.357406744336586));
#19532=DIRECTION('center_axis',(0.707106781186553,0.,0.707106781186542));
#19533=DIRECTION('ref_axis',(0.707106781186542,0.,-0.707106781186553));
#19534=DIRECTION('',(-0.357406744336592,-0.862856209461016,0.357406744336597));
#19535=DIRECTION('',(0.,1.,0.));
#19536=DIRECTION('',(0.707106781186542,0.,-0.707106781186553));
#19537=DIRECTION('',(0.,-1.,0.));
#19538=DIRECTION('center_axis',(0.923879532511287,-0.382683432365088,0.));
#19539=DIRECTION('ref_axis',(0.,0.,-1.));
#19540=DIRECTION('',(0.,0.,-1.));
#19541=DIRECTION('',(0.281084637714813,0.678598344545841,0.678598344545856));
#19542=DIRECTION('',(0.,0.,1.));
#19543=DIRECTION('center_axis',(0.,-0.707106781186546,0.707106781186549));
#19544=DIRECTION('ref_axis',(1.,0.,0.));
#19545=DIRECTION('',(-0.577350269189625,0.577350269189627,0.577350269189625));
#19546=DIRECTION('',(-1.,0.,0.));
#19547=DIRECTION('',(-0.577350269189625,-0.577350269189627,-0.577350269189625));
#19548=DIRECTION('center_axis',(0.,-0.382683432365108,-0.923879532511279));
#19549=DIRECTION('ref_axis',(-1.,0.,0.));
#19550=DIRECTION('',(1.,0.,0.));
#19551=DIRECTION('',(0.678598344545848,-0.678598344545845,0.281084637714824));
#19552=DIRECTION('',(-1.,0.,0.));
#19553=DIRECTION('',(0.678598344545848,0.678598344545845,-0.281084637714824));
#19554=DIRECTION('center_axis',(0.382683432365094,0.,-0.923879532511285));
#19555=DIRECTION('ref_axis',(-0.923879532511285,0.,-0.382683432365094));
#19556=DIRECTION('',(0.,1.,0.));
#19557=DIRECTION('',(0.862856209461013,0.357406744336599,0.357406744336596));
#19558=DIRECTION('',(0.,-1.,0.));
#19559=DIRECTION('center_axis',(-0.382683432365094,0.,-0.923879532511285));
#19560=DIRECTION('ref_axis',(-0.923879532511285,0.,0.382683432365094));
#19561=DIRECTION('',(0.,1.,0.));
#19562=DIRECTION('',(0.862856209461013,-0.357406744336599,-0.357406744336596));
#19563=DIRECTION('',(0.,-1.,0.));
#19564=DIRECTION('center_axis',(0.,0.,-1.));
#19565=DIRECTION('ref_axis',(0.,1.,0.));
#19566=DIRECTION('',(-1.,0.,0.));
#19567=DIRECTION('center_axis',(0.,0.,1.));
#19568=DIRECTION('ref_axis',(1.,0.,0.));
#19569=DIRECTION('center_axis',(0.,0.,1.));
#19570=DIRECTION('ref_axis',(1.,0.,0.));
#19571=DIRECTION('',(-1.,0.,0.));
#19572=DIRECTION('',(-0.769134655216721,-0.639086756352105,0.));
#19573=DIRECTION('center_axis',(0.,0.,-1.));
#19574=DIRECTION('ref_axis',(1.,0.,0.));
#19575=DIRECTION('center_axis',(0.,0.,-1.));
#19576=DIRECTION('ref_axis',(1.,0.,0.));
#19577=DIRECTION('',(0.,0.,1.));
#19578=DIRECTION('center_axis',(0.,0.707106781186545,-0.70710678118655));
#19579=DIRECTION('ref_axis',(0.,-0.70710678118655,-0.707106781186545));
#19580=DIRECTION('center_axis',(0.,0.,1.));
#19581=DIRECTION('ref_axis',(1.,0.,0.));
#19582=DIRECTION('center_axis',(0.,0.707106781186545,-0.70710678118655));
#19583=DIRECTION('ref_axis',(0.,-0.70710678118655,-0.707106781186545));
#19584=DIRECTION('center_axis',(0.,1.,0.));
#19585=DIRECTION('ref_axis',(0.,0.,1.));
#19586=DIRECTION('',(0.,1.,0.));
#19587=DIRECTION('center_axis',(0.,0.,-1.));
#19588=DIRECTION('ref_axis',(1.,0.,0.));
#19589=DIRECTION('center_axis',(0.,0.,-1.));
#19590=DIRECTION('ref_axis',(1.,0.,0.));
#19591=DIRECTION('center_axis',(0.,-1.40939970598124E-15,1.));
#19592=DIRECTION('ref_axis',(1.,-3.03431454927927E-17,0.));
#19593=DIRECTION('center_axis',(0.,0.,1.));
#19594=DIRECTION('ref_axis',(1.,-6.12323399573677E-17,0.));
#19595=DIRECTION('',(-0.382683432365084,-1.2436385183643E-15,0.923879532511289));
#19596=DIRECTION('center_axis',(0.,0.,1.));
#19597=DIRECTION('ref_axis',(1.,0.,0.));
#19598=DIRECTION('center_axis',(0.,0.,-1.));
#19599=DIRECTION('ref_axis',(1.,-6.12323399573677E-17,0.));
#19600=DIRECTION('',(-0.707106781186549,8.65956056235495E-17,0.707106781186546));
#19601=DIRECTION('',(-0.123383141009019,0.711881246125774,-0.691376664293179));
#19602=DIRECTION('center_axis',(0.,0.,1.));
#19603=DIRECTION('ref_axis',(1.,0.,0.));
#19604=DIRECTION('center_axis',(0.,0.,1.));
#19605=DIRECTION('ref_axis',(1.,0.,0.));
#19606=DIRECTION('',(0.,0.,1.));
#19607=DIRECTION('center_axis',(0.,0.,1.));
#19608=DIRECTION('ref_axis',(1.,0.,0.));
#19609=DIRECTION('center_axis',(0.,3.38073055552685E-15,1.));
#19610=DIRECTION('ref_axis',(1.,-3.13005026890514E-17,0.));
#19611=DIRECTION('',(0.92387953251129,-1.20952485545349E-15,-0.382683432365083));
#19612=DIRECTION('center_axis',(0.,0.,1.));
#19613=DIRECTION('ref_axis',(1.,0.,0.));
#19614=DIRECTION('center_axis',(0.,0.,1.));
#19615=DIRECTION('ref_axis',(1.,0.,0.));
#19616=DIRECTION('center_axis',(0.,0.,-1.));
#19617=DIRECTION('ref_axis',(1.,0.,0.));
#19618=DIRECTION('center_axis',(0.,-0.923879532511289,-0.382683432365084));
#19619=DIRECTION('ref_axis',(0.,0.382683432365084,-0.923879532511289));
#19620=DIRECTION('',(1.,0.,0.));
#19621=DIRECTION('',(-0.678598344545838,-0.281084637714822,0.678598344545856));
#19622=DIRECTION('',(-1.,0.,0.));
#19623=DIRECTION('',(-0.678598344545838,0.281084637714822,-0.678598344545856));
#19624=DIRECTION('center_axis',(0.,-0.923879532511289,0.382683432365084));
#19625=DIRECTION('ref_axis',(0.,-0.382683432365084,-0.923879532511289));
#19626=DIRECTION('',(1.,0.,0.));
#19627=DIRECTION('',(0.678598344545835,0.28108463771482,0.678598344545859));
#19628=DIRECTION('',(0.678598344545835,-0.28108463771482,-0.678598344545859));
#19629=DIRECTION('center_axis',(0.382683432365093,-0.923879532511285,0.));
#19630=DIRECTION('ref_axis',(0.,0.,-1.));
#19631=DIRECTION('',(0.,0.,1.));
#19632=DIRECTION('',(0.,0.,-1.));
#19633=DIRECTION('center_axis',(-0.382683432365093,-0.923879532511285,0.));
#19634=DIRECTION('ref_axis',(0.,0.,-1.));
#19635=DIRECTION('',(0.,0.,-1.));
#19636=DIRECTION('',(0.,0.,1.));
#19637=DIRECTION('center_axis',(-0.707106781186549,-0.707106781186546,0.));
#19638=DIRECTION('ref_axis',(0.,0.,1.));
#19639=DIRECTION('',(0.,0.,1.));
#19640=DIRECTION('',(-0.577350269189625,0.577350269189628,0.577350269189625));
#19641=DIRECTION('',(0.577350269189624,-0.577350269189627,0.577350269189627));
#19642=DIRECTION('center_axis',(0.,-1.,0.));
#19643=DIRECTION('ref_axis',(0.,0.,-1.));
#19644=DIRECTION('center_axis',(0.707106781186542,0.,0.707106781186553));
#19645=DIRECTION('ref_axis',(0.707106781186553,0.,-0.707106781186542));
#19646=DIRECTION('',(0.577350269189628,0.577350269189631,-0.577350269189619));
#19647=DIRECTION('',(0.,1.,0.));
#19648=DIRECTION('',(-0.577350269189628,0.57735026918963,0.577350269189619));
#19649=DIRECTION('',(-0.577350269189634,-0.577350269189618,0.577350269189626));
#19650=DIRECTION('',(0.,-1.,0.));
#19651=DIRECTION('',(0.577350269189634,-0.577350269189617,-0.577350269189626));
#19652=DIRECTION('center_axis',(0.707106781186549,-0.707106781186546,0.));
#19653=DIRECTION('ref_axis',(0.,0.,-1.));
#19654=DIRECTION('',(-0.577350269189621,-0.577350269189624,-0.577350269189632));
#19655=DIRECTION('',(-0.357406744336593,-0.357406744336595,-0.862856209461016));
#19656=DIRECTION('',(0.,0.,-1.));
#19657=DIRECTION('',(0.707106781186546,0.707106781186549,0.));
#19658=DIRECTION('',(0.,0.,1.));
#19659=DIRECTION('center_axis',(0.,-0.707106781186553,0.707106781186542));
#19660=DIRECTION('ref_axis',(1.,0.,0.));
#19661=DIRECTION('',(-1.,0.,0.));
#19662=DIRECTION('',(0.577350269189634,0.577350269189617,0.577350269189626));
#19663=DIRECTION('',(-0.577350269189621,0.577350269189624,0.577350269189632));
#19664=DIRECTION('',(-1.,0.,0.));
#19665=DIRECTION('center_axis',(0.,0.,1.));
#19666=DIRECTION('ref_axis',(0.,-1.,0.));
#19667=DIRECTION('',(1.,0.,0.));
#19668=DIRECTION('',(0.,1.,0.));
#19669=DIRECTION('center_axis',(0.923879532511292,0.,-0.382683432365077));
#19670=DIRECTION('ref_axis',(-0.382683432365077,0.,-0.923879532511292));
#19671=DIRECTION('',(0.,1.,0.));
#19672=DIRECTION('',(0.357406744336583,-0.357406744336584,0.862856209461025));
#19673=DIRECTION('',(0.,-1.,0.));
#19674=DIRECTION('center_axis',(0.707106781186549,0.707106781186546,0.));
#19675=DIRECTION('ref_axis',(0.,0.,-1.));
#19676=DIRECTION('',(0.,0.,-1.));
#19677=DIRECTION('',(0.577350269189625,-0.577350269189628,0.577350269189625));
#19678=DIRECTION('',(-0.577350269189626,0.577350269189628,0.577350269189624));
#19679=DIRECTION('',(0.,0.,-1.));
#19680=DIRECTION('',(0.577350269189622,-0.577350269189624,0.577350269189632));
#19681=DIRECTION('center_axis',(0.707106781186548,0.,-0.707106781186548));
#19682=DIRECTION('ref_axis',(-0.707106781186548,0.,-0.707106781186548));
#19683=DIRECTION('',(0.577350269189625,0.577350269189628,0.577350269189625));
#19684=DIRECTION('',(-0.577350269189625,-0.577350269189628,-0.577350269189625));
#19685=DIRECTION('',(-0.577350269189626,0.577350269189626,-0.577350269189626));
#19686=DIRECTION('center_axis',(0.707106781186549,-0.707106781186546,0.));
#19687=DIRECTION('ref_axis',(0.,0.,-1.));
#19688=DIRECTION('',(0.577350269189624,0.577350269189627,-0.577350269189627));
#19689=DIRECTION('center_axis',(-0.923879532511292,0.,-0.382683432365077));
#19690=DIRECTION('ref_axis',(-0.382683432365077,0.,0.923879532511292));
#19691=DIRECTION('',(0.,1.,0.));
#19692=DIRECTION('',(0.357406744336583,0.357406744336584,-0.862856209461025));
#19693=DIRECTION('',(0.,-1.,0.));
#19694=DIRECTION('',(-0.281084637714813,0.678598344545841,0.678598344545856));
#19695=DIRECTION('center_axis',(-0.923879532511287,-0.382683432365088,0.));
#19696=DIRECTION('ref_axis',(0.,0.,1.));
#19697=DIRECTION('',(-0.357406744336592,0.862856209461016,-0.357406744336597));
#19698=DIRECTION('',(0.,0.,-1.));
#19699=DIRECTION('center_axis',(-0.707106781186549,0.707106781186546,0.));
#19700=DIRECTION('ref_axis',(0.,0.,1.));
#19701=DIRECTION('',(0.,0.,1.));
#19702=DIRECTION('',(-0.577350269189628,-0.57735026918963,-0.577350269189619));
#19703=DIRECTION('',(0.577350269189622,0.577350269189624,-0.577350269189632));
#19704=DIRECTION('',(0.,0.,1.));
#19705=DIRECTION('',(-0.577350269189626,-0.577350269189628,-0.577350269189624));
#19706=DIRECTION('',(0.577350269189625,0.577350269189628,-0.577350269189625));
#19707=DIRECTION('center_axis',(-1.,0.,0.));
#19708=DIRECTION('ref_axis',(0.,0.,1.));
#19709=DIRECTION('',(0.,-1.,0.));
#19710=DIRECTION('center_axis',(-1.,0.,0.));
#19711=DIRECTION('ref_axis',(0.,0.707106781186549,-0.707106781186546));
#19712=DIRECTION('',(0.,0.,-1.));
#19713=DIRECTION('',(0.,-1.,0.));
#19714=DIRECTION('center_axis',(-0.707106781186553,0.,0.707106781186542));
#19715=DIRECTION('ref_axis',(0.707106781186542,0.,0.707106781186553));
#19716=DIRECTION('',(0.,1.,0.));
#19717=DIRECTION('',(-0.707106781186542,0.,-0.707106781186553));
#19718=DIRECTION('center_axis',(-0.707106781186542,0.,0.707106781186553));
#19719=DIRECTION('ref_axis',(0.707106781186553,0.,0.707106781186542));
#19720=DIRECTION('',(0.577350269189628,-0.577350269189631,0.577350269189619));
#19721=DIRECTION('',(-0.577350269189634,0.577350269189618,-0.577350269189626));
#19722=DIRECTION('center_axis',(-0.707106781186549,-0.707106781186546,0.));
#19723=DIRECTION('ref_axis',(0.,0.,1.));
#19724=DIRECTION('',(-0.707106781186542,0.707106781186553,0.));
#19725=DIRECTION('',(0.,0.,1.));
#19726=DIRECTION('',(-0.357406744336593,0.357406744336595,0.862856209461016));
#19727=DIRECTION('center_axis',(-0.382683432365088,-0.923879532511288,0.));
#19728=DIRECTION('ref_axis',(0.,0.,-1.));
#19729=DIRECTION('',(0.,0.,1.));
#19730=DIRECTION('',(-0.862856209461024,0.357406744336595,-0.357406744336574));
#19731=DIRECTION('',(0.,0.,-1.));
#19732=DIRECTION('',(0.862856209461024,-0.357406744336595,-0.357406744336574));
#19733=DIRECTION('center_axis',(0.38268343236509,-0.923879532511287,0.));
#19734=DIRECTION('ref_axis',(0.,0.,-1.));
#19735=DIRECTION('',(0.,0.,-1.));
#19736=DIRECTION('',(0.862856209461024,0.357406744336597,0.357406744336571));
#19737=DIRECTION('',(0.,0.,1.));
#19738=DIRECTION('',(-0.862856209461024,-0.357406744336597,0.357406744336571));
#19739=DIRECTION('center_axis',(0.,-0.70710678118654,0.707106781186555));
#19740=DIRECTION('ref_axis',(1.,0.,0.));
#19741=DIRECTION('',(-1.,0.,0.));
#19742=DIRECTION('',(-0.57735026918963,-0.57735026918963,-0.577350269189618));
#19743=DIRECTION('',(1.,0.,0.));
#19744=DIRECTION('',(-0.57735026918963,0.57735026918963,0.577350269189618));
#19745=DIRECTION('center_axis',(0.,-0.70710678118654,-0.707106781186555));
#19746=DIRECTION('ref_axis',(-1.,0.,0.));
#19747=DIRECTION('',(-1.,0.,0.));
#19748=DIRECTION('',(0.57735026918963,0.57735026918963,-0.577350269189618));
#19749=DIRECTION('',(1.,0.,0.));
#19750=DIRECTION('',(0.57735026918963,-0.57735026918963,0.577350269189618));
#19751=DIRECTION('center_axis',(0.,0.,1.));
#19752=DIRECTION('ref_axis',(1.,0.,0.));
#19753=DIRECTION('',(-0.707106781186547,-0.707106781186548,0.));
#19754=DIRECTION('',(-0.707106781186547,0.707106781186548,0.));
#19755=DIRECTION('center_axis',(-0.707106781186548,0.707106781186547,0.));
#19756=DIRECTION('ref_axis',(-0.707106781186547,-0.707106781186548,0.));
#19757=DIRECTION('',(-0.707106781186547,-0.707106781186548,0.));
#19758=DIRECTION('',(0.,0.,1.));
#19759=DIRECTION('center_axis',(0.,-1.,0.));
#19760=DIRECTION('ref_axis',(0.,0.,-1.));
#19761=DIRECTION('',(-1.,0.,0.));
#19762=DIRECTION('',(1.,0.,0.));
#19763=DIRECTION('center_axis',(0.,-1.,0.));
#19764=DIRECTION('ref_axis',(1.,0.,0.));
#19765=DIRECTION('center_axis',(0.,-1.,0.));
#19766=DIRECTION('ref_axis',(0.,0.,1.));
#19767=DIRECTION('center_axis',(0.,-1.,0.));
#19768=DIRECTION('ref_axis',(1.,0.,0.));
#19769=DIRECTION('center_axis',(0.,-1.,0.));
#19770=DIRECTION('ref_axis',(0.,0.,1.));
#19771=DIRECTION('center_axis',(0.,-1.,0.));
#19772=DIRECTION('ref_axis',(1.,0.,0.));
#19773=DIRECTION('',(0.923879532511286,0.382683432365092,1.1314261122877E-16));
#19774=DIRECTION('center_axis',(0.,1.,0.));
#19775=DIRECTION('ref_axis',(1.,0.,0.));
#19776=DIRECTION('center_axis',(0.,-1.,0.));
#19777=DIRECTION('ref_axis',(1.,0.,0.));
#19778=DIRECTION('',(-0.707106781186547,-0.707106781186548,-8.65956056235493E-17));
#19779=DIRECTION('center_axis',(0.,-1.,0.));
#19780=DIRECTION('ref_axis',(0.,0.,1.));
#19781=DIRECTION('',(-8.65956056235497E-17,0.707106781186544,0.707106781186551));
#19782=DIRECTION('center_axis',(0.,1.,0.));
#19783=DIRECTION('ref_axis',(0.,0.,1.));
#19784=DIRECTION('center_axis',(0.,1.,0.));
#19785=DIRECTION('ref_axis',(0.,0.,1.));
#19786=DIRECTION('',(0.,1.,0.));
#19787=DIRECTION('center_axis',(0.,-1.,0.));
#19788=DIRECTION('ref_axis',(0.,0.,1.));
#19789=DIRECTION('center_axis',(0.,-1.,0.));
#19790=DIRECTION('ref_axis',(0.,0.,1.));
#19791=DIRECTION('',(-8.65956056235484E-17,0.707106781186555,0.70710678118654));
#19792=DIRECTION('center_axis',(0.,1.,0.));
#19793=DIRECTION('ref_axis',(0.,0.,1.));
#19794=DIRECTION('center_axis',(0.,1.,0.));
#19795=DIRECTION('ref_axis',(0.,0.,1.));
#19796=DIRECTION('',(0.,1.,0.));
#19797=DIRECTION('center_axis',(0.,-1.,0.));
#19798=DIRECTION('ref_axis',(0.,0.,1.));
#19799=DIRECTION('center_axis',(-1.,0.,0.));
#19800=DIRECTION('ref_axis',(0.,0.707106781186549,-0.707106781186546));
#19801=DIRECTION('center_axis',(1.,0.,0.));
#19802=DIRECTION('ref_axis',(0.,0.707106781186549,-0.707106781186546));
#19803=DIRECTION('center_axis',(0.,-0.923879532511286,0.382683432365092));
#19804=DIRECTION('ref_axis',(0.,-0.382683432365092,-0.923879532511286));
#19805=DIRECTION('center_axis',(1.,0.,0.));
#19806=DIRECTION('ref_axis',(0.,0.707106781186549,-0.707106781186546));
#19807=DIRECTION('center_axis',(-1.,0.,0.));
#19808=DIRECTION('ref_axis',(0.,0.707106781186549,-0.707106781186546));
#19809=DIRECTION('center_axis',(1.,0.,0.));
#19810=DIRECTION('ref_axis',(0.,0.707106781186549,-0.707106781186546));
#19811=DIRECTION('center_axis',(1.,0.,0.));
#19812=DIRECTION('ref_axis',(0.,0.,-1.));
#19813=DIRECTION('center_axis',(0.,-1.,0.));
#19814=DIRECTION('ref_axis',(1.,3.57124208663036E-17,0.));
#19815=DIRECTION('center_axis',(-7.26211808683936E-17,1.,-5.44658856512952E-17));
#19816=DIRECTION('ref_axis',(1.,7.26211808683936E-17,0.));
#19817=DIRECTION('',(-0.923879532511285,-0.382683432365094,1.1314261122877E-16));
#19818=DIRECTION('center_axis',(0.,-1.,0.));
#19819=DIRECTION('ref_axis',(1.,0.,0.));
#19820=DIRECTION('',(0.707106781186548,0.707106781186547,8.65956056235494E-17));
#19821=DIRECTION('center_axis',(7.29827365498645E-17,-1.,-2.00702525512128E-16));
#19822=DIRECTION('ref_axis',(1.,7.29827365498645E-17,0.));
#19823=DIRECTION('center_axis',(0.,1.,0.));
#19824=DIRECTION('ref_axis',(0.,0.,1.));
#19825=DIRECTION('center_axis',(0.,1.,0.));
#19826=DIRECTION('ref_axis',(0.,0.,1.));
#19827=DIRECTION('',(8.65956056235496E-17,-0.707106781186545,0.70710678118655));
#19828=DIRECTION('center_axis',(0.,1.,0.));
#19829=DIRECTION('ref_axis',(0.,0.,1.));
#19830=DIRECTION('',(1.,0.,0.));
#19831=DIRECTION('',(0.,0.,-1.));
#19832=DIRECTION('',(-1.,0.,0.));
#19833=DIRECTION('',(0.,0.,1.));
#19834=DIRECTION('center_axis',(0.,1.,0.));
#19835=DIRECTION('ref_axis',(0.,0.,1.));
#19836=DIRECTION('center_axis',(0.,1.,0.));
#19837=DIRECTION('ref_axis',(1.,0.,0.));
#19838=DIRECTION('center_axis',(0.,1.,0.));
#19839=DIRECTION('ref_axis',(0.,0.,1.));
#19840=DIRECTION('',(8.65956056235484E-17,-0.707106781186555,0.70710678118654));
#19841=DIRECTION('center_axis',(0.,0.923879532511296,0.382683432365068));
#19842=DIRECTION('ref_axis',(0.,-0.382683432365068,0.923879532511296));
#19843=DIRECTION('',(1.,0.,0.));
#19844=DIRECTION('',(-0.678598344545828,0.281084637714811,-0.67859834454587));
#19845=DIRECTION('',(-0.678598344545828,-0.281084637714811,0.67859834454587));
#19846=DIRECTION('center_axis',(0.,0.923879532511288,-0.382683432365088));
#19847=DIRECTION('ref_axis',(0.,0.382683432365088,0.923879532511288));
#19848=DIRECTION('',(0.678598344545841,-0.281084637714821,-0.678598344545853));
#19849=DIRECTION('',(-1.,0.,0.));
#19850=DIRECTION('',(0.678598344545841,0.281084637714821,0.678598344545853));
#19851=DIRECTION('center_axis',(0.382683432365095,0.923879532511285,0.));
#19852=DIRECTION('ref_axis',(0.,0.,1.));
#19853=DIRECTION('center_axis',(-0.382683432365095,0.923879532511285,0.));
#19854=DIRECTION('ref_axis',(0.,0.,1.));
#19855=DIRECTION('center_axis',(0.,0.707106781186545,-0.70710678118655));
#19856=DIRECTION('ref_axis',(-1.,0.,0.));
#19857=DIRECTION('',(-1.,0.,0.));
#19858=DIRECTION('',(0.577350269189625,-0.577350269189628,-0.577350269189625));
#19859=DIRECTION('center_axis',(0.,-1.,0.));
#19860=DIRECTION('ref_axis',(1.,3.67475894571974E-17,0.));
#19861=DIRECTION('',(0.38268343236509,0.923879532511286,4.68652040532631E-17));
#19862=DIRECTION('center_axis',(0.,1.,0.));
#19863=DIRECTION('ref_axis',(1.,0.,0.));
#19864=DIRECTION('center_axis',(0.,-1.,0.));
#19865=DIRECTION('ref_axis',(1.,0.,0.));
#19866=DIRECTION('center_axis',(0.,-1.,0.));
#19867=DIRECTION('ref_axis',(1.,0.,0.));
#19868=DIRECTION('',(0.,-1.,0.));
#19869=DIRECTION('center_axis',(-5.23364152894587E-15,1.,0.));
#19870=DIRECTION('ref_axis',(1.,0.,0.));
#19871=DIRECTION('center_axis',(0.,-1.,-7.26211808683936E-17));
#19872=DIRECTION('ref_axis',(1.,0.,0.));
#19873=DIRECTION('',(-0.923879532511287,0.38268343236509,-1.1314261122877E-16));
#19874=DIRECTION('center_axis',(0.,1.,0.));
#19875=DIRECTION('ref_axis',(1.,0.,0.));
#19876=DIRECTION('',(0.707106781186547,-0.707106781186547,-8.65956056235493E-17));
#19877=DIRECTION('center_axis',(0.,1.,1.45965473099729E-16));
#19878=DIRECTION('ref_axis',(1.,0.,0.));
#19879=DIRECTION('center_axis',(2.16784530188845E-15,1.,0.));
#19880=DIRECTION('ref_axis',(1.,0.,0.));
#19881=DIRECTION('',(0.382683432365085,-0.923879532511289,-4.68652040532626E-17));
#19882=DIRECTION('center_axis',(0.707106781186548,0.707106781186547,0.));
#19883=DIRECTION('ref_axis',(-0.707106781186547,0.707106781186548,0.));
#19884=DIRECTION('',(-0.707106781186547,0.707106781186548,0.));
#19885=DIRECTION('center_axis',(0.,0.,1.));
#19886=DIRECTION('ref_axis',(1.,0.,0.));
#19887=DIRECTION('center_axis',(0.,0.,-1.));
#19888=DIRECTION('ref_axis',(1.,0.,0.));
#19889=DIRECTION('',(0.707106781186547,-8.65956056235493E-17,0.707106781186547));
#19890=DIRECTION('center_axis',(0.,0.,1.));
#19891=DIRECTION('ref_axis',(1.,0.,0.));
#19892=DIRECTION('center_axis',(0.,0.,1.));
#19893=DIRECTION('ref_axis',(1.,0.,0.));
#19894=DIRECTION('center_axis',(0.,-0.707106781186548,-0.707106781186548));
#19895=DIRECTION('ref_axis',(-1.,0.,0.));
#19896=DIRECTION('',(-0.577350269189626,-0.577350269189626,0.577350269189626));
#19897=DIRECTION('center_axis',(-0.707106781186548,0.,-0.707106781186548));
#19898=DIRECTION('ref_axis',(-0.707106781186548,0.,0.707106781186548));
#19899=DIRECTION('center_axis',(0.,0.707106781186552,0.707106781186543));
#19900=DIRECTION('ref_axis',(1.,0.,0.));
#19901=DIRECTION('center_axis',(0.,0.,1.));
#19902=DIRECTION('ref_axis',(0.,-1.,0.));
#19903=DIRECTION('',(1.,0.,0.));
#19904=DIRECTION('center_axis',(1.,0.,0.));
#19905=DIRECTION('ref_axis',(0.,0.707106781186549,-0.707106781186546));
#19906=DIRECTION('axis',(0.,0.,1.));
#19907=DIRECTION('refdir',(1.,0.,0.));
#19908=DIRECTION('center_axis',(0.,0.,1.));
#19909=DIRECTION('ref_axis',(1.,0.,0.));
#19910=DIRECTION('',(0.,0.,-1.));
#19911=DIRECTION('center_axis',(0.,0.,1.));
#19912=DIRECTION('ref_axis',(1.,0.,0.));
#19913=DIRECTION('center_axis',(0.,0.,1.));
#19914=DIRECTION('ref_axis',(1.,0.,0.));
#19915=DIRECTION('',(0.,0.,-1.));
#19916=DIRECTION('center_axis',(0.,0.,1.));
#19917=DIRECTION('ref_axis',(1.,0.,0.));
#19918=DIRECTION('',(0.,0.,-1.));
#19919=DIRECTION('center_axis',(0.,0.,1.));
#19920=DIRECTION('ref_axis',(1.,0.,0.));
#19921=DIRECTION('',(0.,0.,-1.));
#19922=DIRECTION('center_axis',(0.,0.,1.));
#19923=DIRECTION('ref_axis',(1.,0.,0.));
#19924=DIRECTION('',(0.,0.,-1.));
#19925=DIRECTION('center_axis',(0.,0.,1.));
#19926=DIRECTION('ref_axis',(1.,0.,0.));
#19927=DIRECTION('',(0.,0.,-1.));
#19928=DIRECTION('center_axis',(0.,0.,1.));
#19929=DIRECTION('ref_axis',(1.,0.,0.));
#19930=DIRECTION('',(0.,0.,-1.));
#19931=DIRECTION('center_axis',(0.,0.,1.));
#19932=DIRECTION('ref_axis',(1.,0.,0.));
#19933=DIRECTION('',(0.,0.,-1.));
#19934=DIRECTION('center_axis',(0.,0.,1.));
#19935=DIRECTION('ref_axis',(1.,0.,0.));
#19936=DIRECTION('',(0.,0.,-1.));
#19937=DIRECTION('center_axis',(0.,0.,1.));
#19938=DIRECTION('ref_axis',(1.,0.,0.));
#19939=DIRECTION('',(0.,0.,-1.));
#19940=DIRECTION('center_axis',(0.,0.,1.));
#19941=DIRECTION('ref_axis',(1.,0.,0.));
#19942=DIRECTION('',(0.,0.,-1.));
#19943=DIRECTION('center_axis',(0.,0.,1.));
#19944=DIRECTION('ref_axis',(1.,0.,0.));
#19945=DIRECTION('',(0.,0.,-1.));
#19946=DIRECTION('center_axis',(0.,0.,1.));
#19947=DIRECTION('ref_axis',(1.,0.,0.));
#19948=DIRECTION('',(0.,0.,-1.));
#19949=DIRECTION('center_axis',(0.,0.,1.));
#19950=DIRECTION('ref_axis',(1.,0.,0.));
#19951=DIRECTION('',(0.,0.,-1.));
#19952=DIRECTION('center_axis',(0.,0.,1.));
#19953=DIRECTION('ref_axis',(1.,0.,0.));
#19954=DIRECTION('',(0.,0.,-1.));
#19955=DIRECTION('center_axis',(0.,0.,1.));
#19956=DIRECTION('ref_axis',(1.,0.,0.));
#19957=DIRECTION('',(0.,0.,-1.));
#19958=DIRECTION('center_axis',(0.,0.,1.));
#19959=DIRECTION('ref_axis',(1.,0.,0.));
#19960=DIRECTION('',(0.,0.,-1.));
#19961=DIRECTION('center_axis',(0.,0.,1.));
#19962=DIRECTION('ref_axis',(1.,0.,0.));
#19963=DIRECTION('',(0.,0.,-1.));
#19964=DIRECTION('center_axis',(0.,0.,1.));
#19965=DIRECTION('ref_axis',(1.,0.,0.));
#19966=DIRECTION('',(0.,0.,-1.));
#19967=DIRECTION('center_axis',(0.,0.,1.));
#19968=DIRECTION('ref_axis',(1.,0.,0.));
#19969=DIRECTION('',(0.,0.,-1.));
#19970=DIRECTION('center_axis',(0.,0.,1.));
#19971=DIRECTION('ref_axis',(1.,0.,0.));
#19972=DIRECTION('',(0.,0.,-1.));
#19973=DIRECTION('center_axis',(0.,0.,1.));
#19974=DIRECTION('ref_axis',(1.,0.,0.));
#19975=DIRECTION('',(0.,0.,-1.));
#19976=DIRECTION('center_axis',(0.,0.,1.));
#19977=DIRECTION('ref_axis',(1.,0.,0.));
#19978=DIRECTION('',(0.,0.,-1.));
#19979=DIRECTION('center_axis',(0.,0.,1.));
#19980=DIRECTION('ref_axis',(1.,0.,0.));
#19981=DIRECTION('',(0.,0.,-1.));
#19982=DIRECTION('center_axis',(0.,0.,1.));
#19983=DIRECTION('ref_axis',(1.,0.,0.));
#19984=DIRECTION('center_axis',(0.,0.,1.));
#19985=DIRECTION('ref_axis',(0.37267613439428,-0.927961474875405,0.));
#19986=DIRECTION('',(0.,0.,1.));
#19987=DIRECTION('center_axis',(0.,0.,1.));
#19988=DIRECTION('ref_axis',(1.,-7.76068732292971E-15,0.));
#19989=DIRECTION('center_axis',(0.,0.,1.));
#19990=DIRECTION('ref_axis',(1.,-7.76068732292971E-15,0.));
#19991=DIRECTION('',(0.,0.,1.));
#19992=DIRECTION('center_axis',(0.,0.,1.));
#19993=DIRECTION('ref_axis',(1.,-7.76068732292971E-15,0.));
#19994=DIRECTION('',(0.,0.,1.));
#19995=DIRECTION('center_axis',(0.,0.,1.));
#19996=DIRECTION('ref_axis',(1.,-7.76068732292971E-15,0.));
#19997=DIRECTION('',(0.,0.,1.));
#19998=DIRECTION('center_axis',(0.,0.,1.));
#19999=DIRECTION('ref_axis',(1.,-7.76068732292971E-15,0.));
#20000=DIRECTION('',(0.,0.,1.));
#20001=DIRECTION('center_axis',(0.,0.,1.));
#20002=DIRECTION('ref_axis',(1.,-7.76068732292971E-15,0.));
#20003=DIRECTION('',(0.,0.,1.));
#20004=DIRECTION('center_axis',(0.,0.,1.));
#20005=DIRECTION('ref_axis',(1.,-7.76068732292971E-15,0.));
#20006=DIRECTION('',(0.,0.,1.));
#20007=DIRECTION('center_axis',(0.,0.,1.));
#20008=DIRECTION('ref_axis',(1.,-7.76068732292971E-15,0.));
#20009=DIRECTION('',(0.,0.,1.));
#20010=DIRECTION('center_axis',(0.,0.,1.));
#20011=DIRECTION('ref_axis',(1.,-7.76068732292971E-15,0.));
#20012=DIRECTION('',(0.,0.,1.));
#20013=DIRECTION('center_axis',(0.,0.,1.));
#20014=DIRECTION('ref_axis',(1.,-7.76068732292971E-15,0.));
#20015=DIRECTION('',(0.,0.,1.));
#20016=DIRECTION('center_axis',(0.,0.,1.));
#20017=DIRECTION('ref_axis',(1.,-7.76068732292971E-15,0.));
#20018=DIRECTION('',(0.,0.,1.));
#20019=DIRECTION('center_axis',(0.,0.,1.));
#20020=DIRECTION('ref_axis',(1.,-7.76068732292971E-15,0.));
#20021=DIRECTION('',(0.,0.,1.));
#20022=DIRECTION('center_axis',(0.,0.,1.));
#20023=DIRECTION('ref_axis',(1.,-7.76068732292971E-15,0.));
#20024=DIRECTION('',(0.,0.,1.));
#20025=DIRECTION('center_axis',(0.,0.,1.));
#20026=DIRECTION('ref_axis',(1.,-7.76068732292971E-15,0.));
#20027=DIRECTION('',(0.,0.,1.));
#20028=DIRECTION('center_axis',(0.,0.,1.));
#20029=DIRECTION('ref_axis',(1.,-7.76068732292971E-15,0.));
#20030=DIRECTION('',(0.,0.,1.));
#20031=DIRECTION('center_axis',(0.,0.,1.));
#20032=DIRECTION('ref_axis',(1.,-7.76068732292971E-15,0.));
#20033=DIRECTION('',(0.,0.,1.));
#20034=DIRECTION('center_axis',(0.,0.,1.));
#20035=DIRECTION('ref_axis',(1.,-7.76068732292971E-15,0.));
#20036=DIRECTION('',(0.,0.,1.));
#20037=DIRECTION('center_axis',(0.,0.,1.));
#20038=DIRECTION('ref_axis',(1.,-7.76068732292971E-15,0.));
#20039=DIRECTION('',(0.,0.,1.));
#20040=DIRECTION('center_axis',(0.,0.,1.));
#20041=DIRECTION('ref_axis',(1.,-7.76068732292971E-15,0.));
#20042=DIRECTION('',(0.,0.,1.));
#20043=DIRECTION('center_axis',(0.,0.,1.));
#20044=DIRECTION('ref_axis',(1.,-7.76068732292971E-15,0.));
#20045=DIRECTION('',(0.,0.,1.));
#20046=DIRECTION('center_axis',(0.,0.,1.));
#20047=DIRECTION('ref_axis',(1.,-7.76068732292971E-15,0.));
#20048=DIRECTION('',(0.,0.,1.));
#20049=DIRECTION('center_axis',(0.,0.,1.));
#20050=DIRECTION('ref_axis',(1.,-7.76068732292971E-15,0.));
#20051=DIRECTION('',(0.,0.,1.));
#20052=DIRECTION('center_axis',(0.,0.,1.));
#20053=DIRECTION('ref_axis',(1.,-7.76068732292971E-15,0.));
#20054=DIRECTION('',(0.,0.,1.));
#20055=DIRECTION('center_axis',(0.,-1.,0.));
#20056=DIRECTION('ref_axis',(-1.,0.,0.));
#20057=DIRECTION('',(-1.,0.,0.));
#20058=DIRECTION('',(0.,0.,-1.));
#20059=DIRECTION('',(-1.,0.,0.));
#20060=DIRECTION('',(0.,0.,-1.));
#20061=DIRECTION('center_axis',(1.,0.,0.));
#20062=DIRECTION('ref_axis',(0.,-1.,0.));
#20063=DIRECTION('',(0.,-1.,0.));
#20064=DIRECTION('',(0.,0.,-1.));
#20065=DIRECTION('',(0.,-1.,0.));
#20066=DIRECTION('center_axis',(0.,1.,0.));
#20067=DIRECTION('ref_axis',(1.,0.,0.));
#20068=DIRECTION('',(1.,0.,0.));
#20069=DIRECTION('',(0.,0.,-1.));
#20070=DIRECTION('',(1.,0.,0.));
#20071=DIRECTION('center_axis',(-1.,0.,0.));
#20072=DIRECTION('ref_axis',(0.,1.,0.));
#20073=DIRECTION('',(0.,1.,0.));
#20074=DIRECTION('',(0.,1.,0.));
#20075=DIRECTION('center_axis',(0.,0.,-1.));
#20076=DIRECTION('ref_axis',(-1.,0.,0.));
#20077=DIRECTION('center_axis',(0.,0.,1.));
#20078=DIRECTION('ref_axis',(1.,0.,0.));
#20079=DIRECTION('center_axis',(0.,0.,1.));
#20080=DIRECTION('ref_axis',(1.,0.,0.));
#20081=DIRECTION('',(0.,0.,1.));
#20082=DIRECTION('center_axis',(0.,0.,1.));
#20083=DIRECTION('ref_axis',(1.,0.,0.));
#20084=DIRECTION('center_axis',(0.,0.,1.));
#20085=DIRECTION('ref_axis',(1.,0.,0.));
#20086=DIRECTION('center_axis',(0.,0.,1.));
#20087=DIRECTION('ref_axis',(1.,0.,0.));
#20088=DIRECTION('center_axis',(0.,0.,1.));
#20089=DIRECTION('ref_axis',(1.,0.,0.));
#20090=DIRECTION('center_axis',(0.,0.,1.));
#20091=DIRECTION('ref_axis',(1.,0.,0.));
#20092=DIRECTION('center_axis',(0.,0.,-1.));
#20093=DIRECTION('ref_axis',(1.,-7.76068732292971E-15,0.));
#20094=DIRECTION('center_axis',(0.,0.,1.));
#20095=DIRECTION('ref_axis',(1.,-7.76068732292971E-15,0.));
#20096=DIRECTION('center_axis',(-0.0382353162534336,0.999268762941682,0.));
#20097=DIRECTION('ref_axis',(0.999268762941682,0.0382353162534336,0.));
#20098=DIRECTION('',(0.,0.,-1.));
#20099=DIRECTION('',(0.,0.,-1.));
#20100=DIRECTION('center_axis',(-0.768185830790291,-0.640226935838403,0.));
#20101=DIRECTION('ref_axis',(-0.640226935838403,0.768185830790291,0.));
#20102=DIRECTION('',(0.,0.,1.));
#20103=DIRECTION('center_axis',(0.371509522684555,0.928429143529378,0.));
#20104=DIRECTION('ref_axis',(0.928429143529378,-0.371509522684555,0.));
#20105=DIRECTION('',(0.,0.,-1.));
#20106=DIRECTION('',(0.,0.,-1.));
#20107=DIRECTION('center_axis',(-0.962176431033494,-0.272427083021583,0.));
#20108=DIRECTION('ref_axis',(-0.272427083021583,0.962176431033494,0.));
#20109=DIRECTION('',(0.,0.,1.));
#20110=DIRECTION('center_axis',(0.717016990092325,0.697055690686865,0.));
#20111=DIRECTION('ref_axis',(0.697055690686865,-0.717016990092325,0.));
#20112=DIRECTION('',(0.,0.,-1.));
#20113=DIRECTION('',(0.,0.,-1.));
#20114=DIRECTION('center_axis',(-0.989797985252547,0.142477887372033,0.));
#20115=DIRECTION('ref_axis',(0.142477887372033,0.989797985252547,0.));
#20116=DIRECTION('',(0.,0.,1.));
#20117=DIRECTION('center_axis',(0.938545706018272,0.345154976372445,0.));
#20118=DIRECTION('ref_axis',(0.345154976372445,-0.938545706018272,0.));
#20119=DIRECTION('',(0.,0.,-1.));
#20120=DIRECTION('',(0.,0.,-1.));
#20121=DIRECTION('center_axis',(-0.84627447578903,0.532747136668047,0.));
#20122=DIRECTION('ref_axis',(0.532747136668047,0.84627447578903,0.));
#20123=DIRECTION('',(0.,0.,1.));
#20124=DIRECTION('center_axis',(0.997791342953596,-0.0664261689912929,0.));
#20125=DIRECTION('ref_axis',(-0.0664261689912929,-0.997791342953596,0.));
#20126=DIRECTION('',(0.,0.,-1.));
#20127=DIRECTION('',(0.,0.,-1.));
#20128=DIRECTION('center_axis',(-0.556422421299341,0.830899566178355,0.));
#20129=DIRECTION('ref_axis',(0.830899566178355,0.556422421299341,0.));
#20130=DIRECTION('',(0.,0.,1.));
#20131=DIRECTION('center_axis',(0.884509792042463,-0.466521626273638,0.));
#20132=DIRECTION('ref_axis',(-0.466521626273638,-0.884509792042463,0.));
#20133=DIRECTION('',(0.,0.,-1.));
#20134=DIRECTION('',(0.,0.,-1.));
#20135=DIRECTION('center_axis',(-0.170359875227987,0.985381912210847,0.));
#20136=DIRECTION('ref_axis',(0.985381912210847,0.170359875227987,0.));
#20137=DIRECTION('',(0.,0.,1.));
#20138=DIRECTION('center_axis',(0.618288462567988,-0.785951256157348,0.));
#20139=DIRECTION('ref_axis',(-0.785951256157348,-0.618288462567988,0.));
#20140=DIRECTION('',(0.,0.,-1.));
#20141=DIRECTION('',(0.,0.,-1.));
#20142=DIRECTION('center_axis',(0.245159440941167,0.969482773708442,0.));
#20143=DIRECTION('ref_axis',(0.969482773708442,-0.245159440941167,0.));
#20144=DIRECTION('',(0.,0.,1.));
#20145=DIRECTION('center_axis',(-0.441368921654257,0.897325735169653,0.));
#20146=DIRECTION('ref_axis',(0.897325735169653,0.441368921654257,0.));
#20147=DIRECTION('',(0.,0.,-1.));
#20148=DIRECTION('',(0.,0.,-1.));
#20149=DIRECTION('center_axis',(-0.441368921654257,-0.897325735169653,0.));
#20150=DIRECTION('ref_axis',(-0.897325735169653,0.441368921654257,0.));
#20151=DIRECTION('',(0.,0.,1.));
#20152=DIRECTION('center_axis',(0.0382353162534307,-0.999268762941682,0.));
#20153=DIRECTION('ref_axis',(-0.999268762941682,-0.0382353162534307,0.));
#20154=DIRECTION('',(0.,0.,-1.));
#20155=DIRECTION('',(0.,0.,-1.));
#20156=DIRECTION('center_axis',(0.768185830790288,0.640226935838407,0.));
#20157=DIRECTION('ref_axis',(0.640226935838407,-0.768185830790288,0.));
#20158=DIRECTION('',(0.,0.,1.));
#20159=DIRECTION('center_axis',(-0.37150952268456,-0.928429143529376,0.));
#20160=DIRECTION('ref_axis',(-0.928429143529376,0.37150952268456,0.));
#20161=DIRECTION('',(0.,0.,-1.));
#20162=DIRECTION('',(0.,0.,-1.));
#20163=DIRECTION('center_axis',(0.962176431033495,0.27242708302158,0.));
#20164=DIRECTION('ref_axis',(0.27242708302158,-0.962176431033495,0.));
#20165=DIRECTION('',(0.,0.,1.));
#20166=DIRECTION('center_axis',(-0.717016990092328,-0.697055690686862,0.));
#20167=DIRECTION('ref_axis',(-0.697055690686862,0.717016990092328,0.));
#20168=DIRECTION('',(0.,0.,-1.));
#20169=DIRECTION('',(0.,0.,-1.));
#20170=DIRECTION('center_axis',(0.989797985252548,-0.142477887372029,0.));
#20171=DIRECTION('ref_axis',(-0.142477887372029,-0.989797985252548,0.));
#20172=DIRECTION('',(0.,0.,1.));
#20173=DIRECTION('center_axis',(-0.938545706018274,-0.34515497637244,0.));
#20174=DIRECTION('ref_axis',(-0.34515497637244,0.938545706018274,0.));
#20175=DIRECTION('',(0.,0.,-1.));
#20176=DIRECTION('',(0.,0.,-1.));
#20177=DIRECTION('center_axis',(0.846274475789033,-0.532747136668042,0.));
#20178=DIRECTION('ref_axis',(-0.532747136668042,-0.846274475789033,0.));
#20179=DIRECTION('',(0.,0.,1.));
#20180=DIRECTION('center_axis',(-0.997791342953596,0.0664261689912958,0.));
#20181=DIRECTION('ref_axis',(0.0664261689912958,0.997791342953596,0.));
#20182=DIRECTION('',(0.,0.,-1.));
#20183=DIRECTION('',(0.,0.,-1.));
#20184=DIRECTION('center_axis',(0.556422421299338,-0.830899566178357,0.));
#20185=DIRECTION('ref_axis',(-0.830899566178357,-0.556422421299338,0.));
#20186=DIRECTION('',(0.,0.,1.));
#20187=DIRECTION('center_axis',(-0.884509792042462,0.466521626273638,0.));
#20188=DIRECTION('ref_axis',(0.466521626273638,0.884509792042462,0.));
#20189=DIRECTION('',(0.,0.,-1.));
#20190=DIRECTION('',(0.,0.,-1.));
#20191=DIRECTION('center_axis',(0.170359875227985,-0.985381912210847,0.));
#20192=DIRECTION('ref_axis',(-0.985381912210847,-0.170359875227985,0.));
#20193=DIRECTION('',(0.,0.,1.));
#20194=DIRECTION('center_axis',(-0.61828846256799,0.785951256157347,0.));
#20195=DIRECTION('ref_axis',(0.785951256157347,0.61828846256799,0.));
#20196=DIRECTION('',(0.,0.,-1.));
#20197=DIRECTION('',(0.,0.,-1.));
#20198=DIRECTION('center_axis',(-0.245159440941167,-0.969482773708442,0.));
#20199=DIRECTION('ref_axis',(-0.969482773708442,0.245159440941167,0.));
#20200=DIRECTION('',(0.,0.,1.));
#20201=DIRECTION('center_axis',(-0.768185830790289,0.640226935838406,0.));
#20202=DIRECTION('ref_axis',(0.640226935838406,0.768185830790289,0.));
#20203=DIRECTION('',(0.,0.,-1.));
#20204=DIRECTION('',(0.,0.,-1.));
#20205=DIRECTION('center_axis',(-0.0382353162534311,-0.999268762941682,
0.));
#20206=DIRECTION('ref_axis',(-0.999268762941682,0.0382353162534311,0.));
#20207=DIRECTION('',(0.,0.,1.));
#20208=DIRECTION('center_axis',(-0.962176431033495,0.27242708302158,0.));
#20209=DIRECTION('ref_axis',(0.27242708302158,0.962176431033495,0.));
#20210=DIRECTION('',(0.,0.,-1.));
#20211=DIRECTION('',(0.,0.,-1.));
#20212=DIRECTION('center_axis',(0.371509522684558,-0.928429143529377,0.));
#20213=DIRECTION('ref_axis',(-0.928429143529377,-0.371509522684558,0.));
#20214=DIRECTION('',(0.,0.,1.));
#20215=DIRECTION('center_axis',(-0.989797985252548,-0.142477887372029,0.));
#20216=DIRECTION('ref_axis',(-0.142477887372029,0.989797985252548,0.));
#20217=DIRECTION('',(0.,0.,-1.));
#20218=DIRECTION('',(0.,0.,-1.));
#20219=DIRECTION('center_axis',(0.717016990092329,-0.697055690686861,0.));
#20220=DIRECTION('ref_axis',(-0.697055690686861,-0.717016990092329,0.));
#20221=DIRECTION('',(0.,0.,1.));
#20222=DIRECTION('center_axis',(-0.846274475789033,-0.532747136668042,0.));
#20223=DIRECTION('ref_axis',(-0.532747136668042,0.846274475789033,0.));
#20224=DIRECTION('',(0.,0.,-1.));
#20225=DIRECTION('',(0.,0.,-1.));
#20226=DIRECTION('center_axis',(0.938545706018273,-0.345154976372442,0.));
#20227=DIRECTION('ref_axis',(-0.345154976372442,-0.938545706018273,0.));
#20228=DIRECTION('',(0.,0.,1.));
#20229=DIRECTION('center_axis',(-0.556422421299338,-0.830899566178357,0.));
#20230=DIRECTION('ref_axis',(-0.830899566178357,0.556422421299338,0.));
#20231=DIRECTION('',(0.,0.,-1.));
#20232=DIRECTION('',(0.,0.,-1.));
#20233=DIRECTION('center_axis',(0.997791342953596,0.066426168991298,0.));
#20234=DIRECTION('ref_axis',(0.066426168991298,-0.997791342953596,0.));
#20235=DIRECTION('',(0.,0.,1.));
#20236=DIRECTION('center_axis',(-0.170359875227984,-0.985381912210847,0.));
#20237=DIRECTION('ref_axis',(-0.985381912210847,0.170359875227984,0.));
#20238=DIRECTION('',(0.,0.,-1.));
#20239=DIRECTION('',(0.,0.,-1.));
#20240=DIRECTION('center_axis',(0.884509792042461,0.466521626273641,0.));
#20241=DIRECTION('ref_axis',(0.466521626273641,-0.884509792042461,0.));
#20242=DIRECTION('',(0.,0.,1.));
#20243=DIRECTION('center_axis',(0.245159440941165,-0.969482773708443,0.));
#20244=DIRECTION('ref_axis',(-0.969482773708443,-0.245159440941165,0.));
#20245=DIRECTION('',(0.,0.,-1.));
#20246=DIRECTION('',(0.,0.,-1.));
#20247=DIRECTION('center_axis',(0.618288462567991,0.785951256157346,0.));
#20248=DIRECTION('ref_axis',(0.785951256157346,-0.618288462567991,0.));
#20249=DIRECTION('',(0.,0.,1.));
#20250=DIRECTION('center_axis',(0.441368921654258,-0.897325735169653,0.));
#20251=DIRECTION('ref_axis',(-0.897325735169653,-0.441368921654258,0.));
#20252=DIRECTION('',(0.,0.,-1.));
#20253=DIRECTION('',(0.,0.,-1.));
#20254=DIRECTION('center_axis',(0.441368921654255,0.897325735169654,0.));
#20255=DIRECTION('ref_axis',(0.897325735169654,-0.441368921654255,0.));
#20256=DIRECTION('',(0.,0.,1.));
#20257=DIRECTION('center_axis',(0.768185830790287,-0.640226935838408,0.));
#20258=DIRECTION('ref_axis',(-0.640226935838408,-0.768185830790287,0.));
#20259=DIRECTION('',(0.,0.,-1.));
#20260=DIRECTION('',(0.,0.,-1.));
#20261=DIRECTION('center_axis',(0.0382353162534311,0.999268762941682,0.));
#20262=DIRECTION('ref_axis',(0.999268762941682,-0.0382353162534311,0.));
#20263=DIRECTION('',(0.,0.,1.));
#20264=DIRECTION('center_axis',(0.962176431033494,-0.272427083021581,0.));
#20265=DIRECTION('ref_axis',(-0.272427083021581,-0.962176431033494,0.));
#20266=DIRECTION('',(0.,0.,-1.));
#20267=DIRECTION('',(0.,0.,-1.));
#20268=DIRECTION('center_axis',(-0.371509522684558,0.928429143529377,0.));
#20269=DIRECTION('ref_axis',(0.928429143529377,0.371509522684558,0.));
#20270=DIRECTION('',(0.,0.,1.));
#20271=DIRECTION('center_axis',(0.989797985252548,0.142477887372027,0.));
#20272=DIRECTION('ref_axis',(0.142477887372027,-0.989797985252548,0.));
#20273=DIRECTION('',(0.,0.,-1.));
#20274=DIRECTION('',(0.,0.,-1.));
#20275=DIRECTION('center_axis',(-0.717016990092329,0.697055690686861,0.));
#20276=DIRECTION('ref_axis',(0.697055690686861,0.717016990092329,0.));
#20277=DIRECTION('',(0.,0.,1.));
#20278=DIRECTION('center_axis',(0.84627447578903,0.532747136668047,0.));
#20279=DIRECTION('ref_axis',(0.532747136668047,-0.84627447578903,0.));
#20280=DIRECTION('',(0.,0.,-1.));
#20281=DIRECTION('',(0.,0.,-1.));
#20282=DIRECTION('center_axis',(-0.938545706018274,0.34515497637244,0.));
#20283=DIRECTION('ref_axis',(0.34515497637244,0.938545706018274,0.));
#20284=DIRECTION('',(0.,0.,1.));
#20285=DIRECTION('center_axis',(0.556422421299336,0.830899566178359,0.));
#20286=DIRECTION('ref_axis',(0.830899566178359,-0.556422421299336,0.));
#20287=DIRECTION('',(0.,0.,-1.));
#20288=DIRECTION('',(0.,0.,-1.));
#20289=DIRECTION('center_axis',(-0.997791342953596,-0.0664261689912929,
0.));
#20290=DIRECTION('ref_axis',(-0.0664261689912929,0.997791342953596,0.));
#20291=DIRECTION('',(0.,0.,1.));
#20292=DIRECTION('center_axis',(0.170359875227981,0.985381912210848,0.));
#20293=DIRECTION('ref_axis',(0.985381912210848,-0.170359875227981,0.));
#20294=DIRECTION('',(0.,0.,-1.));
#20295=DIRECTION('',(0.,0.,-1.));
#20296=DIRECTION('center_axis',(-0.884509792042464,-0.466521626273636,0.));
#20297=DIRECTION('ref_axis',(-0.466521626273636,0.884509792042464,0.));
#20298=DIRECTION('',(0.,0.,1.));
#20299=DIRECTION('center_axis',(-0.24515944094117,0.969482773708441,0.));
#20300=DIRECTION('ref_axis',(0.969482773708441,0.24515944094117,0.));
#20301=DIRECTION('',(0.,0.,-1.));
#20302=DIRECTION('',(0.,0.,-1.));
#20303=DIRECTION('center_axis',(-0.618288462567989,-0.785951256157348,0.));
#20304=DIRECTION('ref_axis',(-0.785951256157348,0.618288462567989,0.));
#20305=DIRECTION('',(0.,0.,1.));
#20306=DIRECTION('center_axis',(0.,0.,1.));
#20307=DIRECTION('ref_axis',(1.,0.,0.));
#20308=DIRECTION('center_axis',(0.,0.,1.));
#20309=DIRECTION('ref_axis',(1.,0.,0.));
#20310=DIRECTION('center_axis',(0.,0.,1.));
#20311=DIRECTION('ref_axis',(1.,0.,0.));
#20312=DIRECTION('center_axis',(0.,0.,1.));
#20313=DIRECTION('ref_axis',(1.,0.,0.));
#20314=DIRECTION('center_axis',(0.,0.,1.));
#20315=DIRECTION('ref_axis',(1.,0.,0.));
#20316=DIRECTION('center_axis',(0.,0.,1.));
#20317=DIRECTION('ref_axis',(1.,0.,0.));
#20318=DIRECTION('center_axis',(0.,0.,1.));
#20319=DIRECTION('ref_axis',(1.,0.,0.));
#20320=DIRECTION('center_axis',(0.,0.,1.));
#20321=DIRECTION('ref_axis',(1.,0.,0.));
#20322=DIRECTION('center_axis',(0.,0.,1.));
#20323=DIRECTION('ref_axis',(1.,0.,0.));
#20324=DIRECTION('center_axis',(0.,0.,1.));
#20325=DIRECTION('ref_axis',(1.,0.,0.));
#20326=DIRECTION('center_axis',(0.,0.,1.));
#20327=DIRECTION('ref_axis',(1.,0.,0.));
#20328=DIRECTION('center_axis',(0.,0.,1.));
#20329=DIRECTION('ref_axis',(1.,0.,0.));
#20330=DIRECTION('center_axis',(0.,0.,1.));
#20331=DIRECTION('ref_axis',(1.,0.,0.));
#20332=DIRECTION('center_axis',(0.,0.,1.));
#20333=DIRECTION('ref_axis',(1.,0.,0.));
#20334=DIRECTION('center_axis',(0.,0.,1.));
#20335=DIRECTION('ref_axis',(1.,0.,0.));
#20336=DIRECTION('center_axis',(0.,0.,1.));
#20337=DIRECTION('ref_axis',(1.,0.,0.));
#20338=DIRECTION('center_axis',(0.,0.,1.));
#20339=DIRECTION('ref_axis',(1.,0.,0.));
#20340=DIRECTION('center_axis',(0.,0.,1.));
#20341=DIRECTION('ref_axis',(1.,0.,0.));
#20342=DIRECTION('center_axis',(0.,0.,1.));
#20343=DIRECTION('ref_axis',(1.,0.,0.));
#20344=DIRECTION('center_axis',(0.,0.,1.));
#20345=DIRECTION('ref_axis',(1.,0.,0.));
#20346=DIRECTION('center_axis',(0.,0.,1.));
#20347=DIRECTION('ref_axis',(1.,0.,0.));
#20348=DIRECTION('center_axis',(0.,0.,1.));
#20349=DIRECTION('ref_axis',(1.,0.,0.));
#20350=DIRECTION('center_axis',(0.,0.,1.));
#20351=DIRECTION('ref_axis',(1.,0.,0.));
#20352=DIRECTION('center_axis',(0.,0.,1.));
#20353=DIRECTION('ref_axis',(1.,0.,0.));
#20354=DIRECTION('center_axis',(0.,0.,1.));
#20355=DIRECTION('ref_axis',(1.,0.,0.));
#20356=DIRECTION('center_axis',(0.,0.,1.));
#20357=DIRECTION('ref_axis',(1.,0.,0.));
#20358=DIRECTION('center_axis',(0.,0.,1.));
#20359=DIRECTION('ref_axis',(1.,0.,0.));
#20360=DIRECTION('center_axis',(0.,0.,1.));
#20361=DIRECTION('ref_axis',(1.,0.,0.));
#20362=DIRECTION('center_axis',(0.,0.,1.));
#20363=DIRECTION('ref_axis',(1.,0.,0.));
#20364=DIRECTION('center_axis',(0.,0.,1.));
#20365=DIRECTION('ref_axis',(1.,0.,0.));
#20366=DIRECTION('center_axis',(0.,0.,1.));
#20367=DIRECTION('ref_axis',(1.,0.,0.));
#20368=DIRECTION('center_axis',(0.,0.,1.));
#20369=DIRECTION('ref_axis',(1.,0.,0.));
#20370=DIRECTION('center_axis',(0.,0.,1.));
#20371=DIRECTION('ref_axis',(1.,0.,0.));
#20372=DIRECTION('center_axis',(0.,0.,1.));
#20373=DIRECTION('ref_axis',(1.,0.,0.));
#20374=DIRECTION('center_axis',(0.,0.,1.));
#20375=DIRECTION('ref_axis',(1.,0.,0.));
#20376=DIRECTION('center_axis',(0.,0.,1.));
#20377=DIRECTION('ref_axis',(1.,0.,0.));
#20378=DIRECTION('center_axis',(0.,0.,1.));
#20379=DIRECTION('ref_axis',(1.,0.,0.));
#20380=DIRECTION('center_axis',(0.,0.,1.));
#20381=DIRECTION('ref_axis',(1.,0.,0.));
#20382=DIRECTION('center_axis',(0.,0.,1.));
#20383=DIRECTION('ref_axis',(1.,0.,0.));
#20384=DIRECTION('center_axis',(0.,0.,1.));
#20385=DIRECTION('ref_axis',(1.,0.,0.));
#20386=DIRECTION('center_axis',(0.,0.,1.));
#20387=DIRECTION('ref_axis',(1.,0.,0.));
#20388=DIRECTION('center_axis',(0.,0.,1.));
#20389=DIRECTION('ref_axis',(1.,0.,0.));
#20390=DIRECTION('center_axis',(0.,0.,1.));
#20391=DIRECTION('ref_axis',(1.,0.,0.));
#20392=DIRECTION('center_axis',(0.,0.,1.));
#20393=DIRECTION('ref_axis',(1.,0.,0.));
#20394=DIRECTION('center_axis',(0.,0.,1.));
#20395=DIRECTION('ref_axis',(1.,0.,0.));
#20396=DIRECTION('center_axis',(0.,0.,1.));
#20397=DIRECTION('ref_axis',(1.,0.,0.));
#20398=DIRECTION('center_axis',(0.,0.,1.));
#20399=DIRECTION('ref_axis',(1.,0.,0.));
#20400=DIRECTION('center_axis',(0.,0.,1.));
#20401=DIRECTION('ref_axis',(1.,0.,0.));
#20402=DIRECTION('center_axis',(0.,0.,1.));
#20403=DIRECTION('ref_axis',(1.,0.,0.));
#20404=DIRECTION('center_axis',(0.,0.,1.));
#20405=DIRECTION('ref_axis',(1.,0.,0.));
#20406=DIRECTION('center_axis',(0.,0.,1.));
#20407=DIRECTION('ref_axis',(1.,0.,0.));
#20408=DIRECTION('center_axis',(0.,0.,1.));
#20409=DIRECTION('ref_axis',(1.,0.,0.));
#20410=DIRECTION('center_axis',(0.,0.,1.));
#20411=DIRECTION('ref_axis',(1.,0.,0.));
#20412=DIRECTION('center_axis',(0.,0.,1.));
#20413=DIRECTION('ref_axis',(1.,0.,0.));
#20414=DIRECTION('center_axis',(0.,0.,1.));
#20415=DIRECTION('ref_axis',(1.,0.,0.));
#20416=DIRECTION('center_axis',(0.,0.,1.));
#20417=DIRECTION('ref_axis',(1.,0.,0.));
#20418=DIRECTION('center_axis',(0.,0.,1.));
#20419=DIRECTION('ref_axis',(1.,0.,0.));
#20420=DIRECTION('center_axis',(0.,0.,1.));
#20421=DIRECTION('ref_axis',(1.,0.,0.));
#20422=DIRECTION('center_axis',(0.,0.,1.));
#20423=DIRECTION('ref_axis',(1.,0.,0.));
#20424=DIRECTION('center_axis',(0.,0.,1.));
#20425=DIRECTION('ref_axis',(1.,0.,0.));
#20426=DIRECTION('center_axis',(0.,0.,1.));
#20427=DIRECTION('ref_axis',(1.,0.,0.));
#20428=DIRECTION('center_axis',(0.,0.,1.));
#20429=DIRECTION('ref_axis',(1.,0.,0.));
#20430=DIRECTION('center_axis',(0.,0.,1.));
#20431=DIRECTION('ref_axis',(1.,0.,0.));
#20432=DIRECTION('center_axis',(0.,0.,1.));
#20433=DIRECTION('ref_axis',(1.,0.,0.));
#20434=DIRECTION('center_axis',(0.,0.,1.));
#20435=DIRECTION('ref_axis',(1.,0.,0.));
#20436=DIRECTION('center_axis',(0.,0.,1.));
#20437=DIRECTION('ref_axis',(1.,0.,0.));
#20438=DIRECTION('center_axis',(0.,0.,1.));
#20439=DIRECTION('ref_axis',(1.,0.,0.));
#20440=DIRECTION('center_axis',(0.,0.,1.));
#20441=DIRECTION('ref_axis',(1.,0.,0.));
#20442=DIRECTION('center_axis',(0.,0.,1.));
#20443=DIRECTION('ref_axis',(1.,0.,0.));
#20444=DIRECTION('center_axis',(0.,0.,1.));
#20445=DIRECTION('ref_axis',(1.,0.,0.));
#20446=DIRECTION('center_axis',(0.,0.,1.));
#20447=DIRECTION('ref_axis',(1.,0.,0.));
#20448=DIRECTION('center_axis',(0.,0.,1.));
#20449=DIRECTION('ref_axis',(1.,0.,0.));
#20450=DIRECTION('center_axis',(0.,0.,1.));
#20451=DIRECTION('ref_axis',(1.,0.,0.));
#20452=DIRECTION('center_axis',(0.,0.,1.));
#20453=DIRECTION('ref_axis',(1.,0.,0.));
#20454=DIRECTION('center_axis',(0.,0.,1.));
#20455=DIRECTION('ref_axis',(1.,0.,0.));
#20456=DIRECTION('center_axis',(0.,0.,1.));
#20457=DIRECTION('ref_axis',(1.,0.,0.));
#20458=DIRECTION('center_axis',(0.,0.,1.));
#20459=DIRECTION('ref_axis',(1.,0.,0.));
#20460=DIRECTION('center_axis',(0.,0.,1.));
#20461=DIRECTION('ref_axis',(1.,0.,0.));
#20462=DIRECTION('center_axis',(0.,0.,1.));
#20463=DIRECTION('ref_axis',(1.,0.,0.));
#20464=DIRECTION('center_axis',(0.,0.,1.));
#20465=DIRECTION('ref_axis',(1.,0.,0.));
#20466=DIRECTION('center_axis',(0.,0.,1.));
#20467=DIRECTION('ref_axis',(1.,0.,0.));
#20468=DIRECTION('center_axis',(0.,0.,1.));
#20469=DIRECTION('ref_axis',(1.,0.,0.));
#20470=DIRECTION('center_axis',(0.,0.,1.));
#20471=DIRECTION('ref_axis',(1.,0.,0.));
#20472=DIRECTION('center_axis',(0.,0.,1.));
#20473=DIRECTION('ref_axis',(1.,0.,0.));
#20474=DIRECTION('center_axis',(0.,0.,1.));
#20475=DIRECTION('ref_axis',(1.,0.,0.));
#20476=DIRECTION('center_axis',(0.,0.,1.));
#20477=DIRECTION('ref_axis',(1.,0.,0.));
#20478=DIRECTION('center_axis',(0.,0.,1.));
#20479=DIRECTION('ref_axis',(1.,0.,0.));
#20480=DIRECTION('center_axis',(0.,0.,1.));
#20481=DIRECTION('ref_axis',(1.,0.,0.));
#20482=DIRECTION('center_axis',(0.,0.,1.));
#20483=DIRECTION('ref_axis',(1.,0.,0.));
#20484=DIRECTION('center_axis',(0.,0.,1.));
#20485=DIRECTION('ref_axis',(1.,0.,0.));
#20486=DIRECTION('center_axis',(0.,0.,1.));
#20487=DIRECTION('ref_axis',(1.,0.,0.));
#20488=DIRECTION('',(0.707106781186547,8.65956056235493E-17,-0.707106781186548));
#20489=DIRECTION('center_axis',(0.,0.,1.));
#20490=DIRECTION('ref_axis',(1.,0.,0.));
#20491=DIRECTION('center_axis',(0.,0.,-1.));
#20492=DIRECTION('ref_axis',(-1.,0.,0.));
#20493=DIRECTION('center_axis',(0.,0.,1.));
#20494=DIRECTION('ref_axis',(1.,0.,0.));
#20495=DIRECTION('center_axis',(0.,0.,1.));
#20496=DIRECTION('ref_axis',(1.,0.,0.));
#20497=DIRECTION('',(0.707106781186547,8.65956056235493E-17,-0.707106781186548));
#20498=DIRECTION('center_axis',(0.,0.,1.));
#20499=DIRECTION('ref_axis',(-0.956376276288062,-0.292137669863679,0.));
#20500=DIRECTION('center_axis',(0.,0.,1.));
#20501=DIRECTION('ref_axis',(1.,0.,0.));
#20502=DIRECTION('center_axis',(0.,0.,-1.));
#20503=DIRECTION('ref_axis',(-1.,0.,0.));
#20504=DIRECTION('center_axis',(0.,0.,-1.));
#20505=DIRECTION('ref_axis',(1.,0.,0.));
#20506=DIRECTION('center_axis',(0.,0.,1.));
#20507=DIRECTION('ref_axis',(1.,0.,0.));
#20508=DIRECTION('',(-0.707106781186548,-8.65956056235493E-17,-0.707106781186547));
#20509=DIRECTION('center_axis',(0.,0.,1.));
#20510=DIRECTION('ref_axis',(1.,0.,0.));
#20511=DIRECTION('axis',(0.,0.,1.));
#20512=DIRECTION('refdir',(1.,0.,0.));
#20513=DIRECTION('center_axis',(6.12323399573677E-17,0.,1.));
#20514=DIRECTION('ref_axis',(1.,0.,0.));
#20515=DIRECTION('center_axis',(1.22464679914735E-16,-1.,0.));
#20516=DIRECTION('ref_axis',(-1.,-1.22464679914735E-16,0.));
#20517=DIRECTION('axis',(0.,0.,1.));
#20518=DIRECTION('refdir',(1.,0.,0.));
#20519=DIRECTION('center_axis',(-0.00361045998153645,0.999206964682131,
0.0396535787722272));
#20520=DIRECTION('ref_axis',(0.000143280351062803,-0.0396533199138007,0.999213487544356));
#20521=DIRECTION('center_axis',(0.00361045998921086,0.999206964681458,0.0396535787884862));
#20522=DIRECTION('ref_axis',(-0.853800279921239,-0.017563245976609,0.520304347855348));
#20523=DIRECTION('center_axis',(0.00361045998921086,0.999206964681458,0.0396535787884862));
#20524=DIRECTION('ref_axis',(-0.853800279921239,-0.017563245976609,0.520304347855348));
#20525=DIRECTION('center_axis',(-0.00361045998153645,0.999206964682131,
0.0396535787722272));
#20526=DIRECTION('ref_axis',(0.000143280351062803,-0.0396533199138007,0.999213487544356));
#20527=DIRECTION('axis',(0.,0.,1.));
#20528=DIRECTION('refdir',(1.,0.,0.));
#20529=DIRECTION('center_axis',(0.,0.,1.));
#20530=DIRECTION('ref_axis',(1.,0.,0.));
#20531=DIRECTION('',(0.,0.,-1.));
#20532=DIRECTION('center_axis',(0.,0.,1.));
#20533=DIRECTION('ref_axis',(1.,0.,0.));
#20534=DIRECTION('center_axis',(0.,0.,1.));
#20535=DIRECTION('ref_axis',(1.,0.,0.));
#20536=DIRECTION('',(0.,0.,-1.));
#20537=DIRECTION('center_axis',(0.,0.,1.));
#20538=DIRECTION('ref_axis',(1.,0.,0.));
#20539=DIRECTION('',(0.,0.,-1.));
#20540=DIRECTION('center_axis',(0.,0.,1.));
#20541=DIRECTION('ref_axis',(1.,0.,0.));
#20542=DIRECTION('',(0.,0.,-1.));
#20543=DIRECTION('center_axis',(0.,0.,1.));
#20544=DIRECTION('ref_axis',(1.,0.,0.));
#20545=DIRECTION('',(0.,0.,-1.));
#20546=DIRECTION('center_axis',(0.,0.,1.));
#20547=DIRECTION('ref_axis',(1.,0.,0.));
#20548=DIRECTION('',(0.,0.,-1.));
#20549=DIRECTION('center_axis',(0.,0.,1.));
#20550=DIRECTION('ref_axis',(1.,0.,0.));
#20551=DIRECTION('',(0.,0.,-1.));
#20552=DIRECTION('center_axis',(0.,0.,1.));
#20553=DIRECTION('ref_axis',(1.,0.,0.));
#20554=DIRECTION('',(0.,0.,-1.));
#20555=DIRECTION('center_axis',(0.,0.,1.));
#20556=DIRECTION('ref_axis',(1.,0.,0.));
#20557=DIRECTION('',(0.,0.,-1.));
#20558=DIRECTION('center_axis',(0.,0.,1.));
#20559=DIRECTION('ref_axis',(1.,0.,0.));
#20560=DIRECTION('',(0.,0.,-1.));
#20561=DIRECTION('center_axis',(0.,0.,1.));
#20562=DIRECTION('ref_axis',(1.,0.,0.));
#20563=DIRECTION('',(0.,0.,-1.));
#20564=DIRECTION('center_axis',(0.,0.,1.));
#20565=DIRECTION('ref_axis',(1.,0.,0.));
#20566=DIRECTION('',(0.,0.,-1.));
#20567=DIRECTION('center_axis',(0.,0.,1.));
#20568=DIRECTION('ref_axis',(1.,0.,0.));
#20569=DIRECTION('',(0.,0.,-1.));
#20570=DIRECTION('center_axis',(0.,0.,1.));
#20571=DIRECTION('ref_axis',(1.,0.,0.));
#20572=DIRECTION('',(0.,0.,-1.));
#20573=DIRECTION('center_axis',(0.,0.,1.));
#20574=DIRECTION('ref_axis',(1.,0.,0.));
#20575=DIRECTION('',(0.,0.,-1.));
#20576=DIRECTION('center_axis',(0.,0.,1.));
#20577=DIRECTION('ref_axis',(1.,0.,0.));
#20578=DIRECTION('',(0.,0.,-1.));
#20579=DIRECTION('center_axis',(0.,0.,1.));
#20580=DIRECTION('ref_axis',(1.,0.,0.));
#20581=DIRECTION('',(0.,0.,-1.));
#20582=DIRECTION('center_axis',(0.,0.,1.));
#20583=DIRECTION('ref_axis',(1.,0.,0.));
#20584=DIRECTION('',(0.,0.,-1.));
#20585=DIRECTION('center_axis',(0.,0.,1.));
#20586=DIRECTION('ref_axis',(1.,0.,0.));
#20587=DIRECTION('',(0.,0.,-1.));
#20588=DIRECTION('center_axis',(0.,0.,1.));
#20589=DIRECTION('ref_axis',(1.,0.,0.));
#20590=DIRECTION('',(0.,0.,-1.));
#20591=DIRECTION('center_axis',(0.,0.,1.));
#20592=DIRECTION('ref_axis',(1.,0.,0.));
#20593=DIRECTION('',(0.,0.,-1.));
#20594=DIRECTION('center_axis',(0.,0.,1.));
#20595=DIRECTION('ref_axis',(1.,0.,0.));
#20596=DIRECTION('',(0.,0.,-1.));
#20597=DIRECTION('center_axis',(0.,0.,1.));
#20598=DIRECTION('ref_axis',(-0.266010414634152,-0.963970154779787,0.));
#20599=DIRECTION('',(0.,0.,1.));
#20600=DIRECTION('center_axis',(0.,0.,1.));
#20601=DIRECTION('ref_axis',(1.,4.93993055488555E-14,0.));
#20602=DIRECTION('center_axis',(0.,0.,1.));
#20603=DIRECTION('ref_axis',(1.,4.93993055488555E-14,0.));
#20604=DIRECTION('',(0.,0.,1.));
#20605=DIRECTION('center_axis',(0.,0.,1.));
#20606=DIRECTION('ref_axis',(1.,4.93993055488555E-14,0.));
#20607=DIRECTION('',(0.,0.,1.));
#20608=DIRECTION('center_axis',(0.,0.,1.));
#20609=DIRECTION('ref_axis',(1.,4.93993055488555E-14,0.));
#20610=DIRECTION('',(0.,0.,1.));
#20611=DIRECTION('center_axis',(0.,0.,1.));
#20612=DIRECTION('ref_axis',(1.,4.93993055488555E-14,0.));
#20613=DIRECTION('',(0.,0.,1.));
#20614=DIRECTION('center_axis',(0.,0.,1.));
#20615=DIRECTION('ref_axis',(1.,4.93993055488555E-14,0.));
#20616=DIRECTION('',(0.,0.,1.));
#20617=DIRECTION('center_axis',(0.,0.,1.));
#20618=DIRECTION('ref_axis',(1.,4.93993055488555E-14,0.));
#20619=DIRECTION('',(0.,0.,1.));
#20620=DIRECTION('center_axis',(0.,0.,1.));
#20621=DIRECTION('ref_axis',(1.,4.93993055488555E-14,0.));
#20622=DIRECTION('',(0.,0.,1.));
#20623=DIRECTION('center_axis',(0.,0.,1.));
#20624=DIRECTION('ref_axis',(1.,4.93993055488555E-14,0.));
#20625=DIRECTION('',(0.,0.,1.));
#20626=DIRECTION('center_axis',(0.,0.,1.));
#20627=DIRECTION('ref_axis',(1.,4.93993055488555E-14,0.));
#20628=DIRECTION('',(0.,0.,1.));
#20629=DIRECTION('center_axis',(0.,0.,1.));
#20630=DIRECTION('ref_axis',(1.,4.93993055488555E-14,0.));
#20631=DIRECTION('',(0.,0.,1.));
#20632=DIRECTION('center_axis',(0.,0.,1.));
#20633=DIRECTION('ref_axis',(1.,4.93993055488555E-14,0.));
#20634=DIRECTION('',(0.,0.,1.));
#20635=DIRECTION('center_axis',(0.,0.,1.));
#20636=DIRECTION('ref_axis',(1.,4.93993055488555E-14,0.));
#20637=DIRECTION('',(0.,0.,1.));
#20638=DIRECTION('center_axis',(0.,0.,1.));
#20639=DIRECTION('ref_axis',(1.,4.93993055488555E-14,0.));
#20640=DIRECTION('',(0.,0.,1.));
#20641=DIRECTION('center_axis',(0.,0.,1.));
#20642=DIRECTION('ref_axis',(1.,4.93993055488555E-14,0.));
#20643=DIRECTION('',(0.,0.,1.));
#20644=DIRECTION('center_axis',(0.,0.,1.));
#20645=DIRECTION('ref_axis',(1.,4.93993055488555E-14,0.));
#20646=DIRECTION('',(0.,0.,1.));
#20647=DIRECTION('center_axis',(0.,0.,1.));
#20648=DIRECTION('ref_axis',(1.,4.93993055488555E-14,0.));
#20649=DIRECTION('',(0.,0.,1.));
#20650=DIRECTION('center_axis',(0.,0.,1.));
#20651=DIRECTION('ref_axis',(1.,4.93993055488555E-14,0.));
#20652=DIRECTION('',(0.,0.,1.));
#20653=DIRECTION('center_axis',(0.,0.,1.));
#20654=DIRECTION('ref_axis',(1.,4.93993055488555E-14,0.));
#20655=DIRECTION('',(0.,0.,1.));
#20656=DIRECTION('center_axis',(0.,0.,1.));
#20657=DIRECTION('ref_axis',(1.,4.93993055488555E-14,0.));
#20658=DIRECTION('',(0.,0.,1.));
#20659=DIRECTION('center_axis',(0.,0.,1.));
#20660=DIRECTION('ref_axis',(1.,4.93993055488555E-14,0.));
#20661=DIRECTION('',(0.,0.,1.));
#20662=DIRECTION('center_axis',(0.,0.,1.));
#20663=DIRECTION('ref_axis',(1.,4.93993055488555E-14,0.));
#20664=DIRECTION('',(0.,0.,1.));
#20665=DIRECTION('center_axis',(0.,0.,1.));
#20666=DIRECTION('ref_axis',(1.,0.,0.));
#20667=DIRECTION('center_axis',(0.,0.,1.));
#20668=DIRECTION('ref_axis',(1.,0.,0.));
#20669=DIRECTION('center_axis',(0.,0.,1.));
#20670=DIRECTION('ref_axis',(1.,0.,0.));
#20671=DIRECTION('center_axis',(0.,0.,1.));
#20672=DIRECTION('ref_axis',(1.,0.,0.));
#20673=DIRECTION('center_axis',(0.,0.,1.));
#20674=DIRECTION('ref_axis',(1.,0.,0.));
#20675=DIRECTION('center_axis',(0.,0.,1.));
#20676=DIRECTION('ref_axis',(1.,0.,0.));
#20677=DIRECTION('center_axis',(0.,0.,-1.));
#20678=DIRECTION('ref_axis',(1.,4.93993055488555E-14,0.));
#20679=DIRECTION('center_axis',(0.,0.,1.));
#20680=DIRECTION('ref_axis',(1.,4.93993055488555E-14,0.));
#20681=DIRECTION('center_axis',(0.,0.,1.));
#20682=DIRECTION('ref_axis',(1.,0.,0.));
#20683=DIRECTION('center_axis',(1.22464679914735E-16,-1.,0.));
#20684=DIRECTION('ref_axis',(-1.,-1.22464679914735E-16,0.));
#20685=DIRECTION('center_axis',(0.,0.,-1.));
#20686=DIRECTION('ref_axis',(1.,0.,0.));
#20687=DIRECTION('center_axis',(0.,0.,1.));
#20688=DIRECTION('ref_axis',(1.,0.,0.));
#20689=DIRECTION('center_axis',(0.,0.,1.));
#20690=DIRECTION('ref_axis',(0.939073012437622,-0.343717729119883,0.));
#20691=DIRECTION('center_axis',(0.,0.,-1.));
#20692=DIRECTION('ref_axis',(-1.,0.,0.));
#20693=DIRECTION('',(-0.999593826304735,-0.0284988142465338,0.));
#20694=DIRECTION('',(0.747414611328346,-0.664357884556884,0.));
#20695=DIRECTION('center_axis',(0.,0.,1.));
#20696=DIRECTION('ref_axis',(1.,0.,0.));
#20697=DIRECTION('',(-0.989356517167622,0.145511793123284,0.));
#20698=DIRECTION('',(0.620695167978805,-0.78405198070521,0.));
#20699=DIRECTION('center_axis',(0.,0.,1.));
#20700=DIRECTION('ref_axis',(1.,0.,0.));
#20701=DIRECTION('',(-0.949058110894924,0.315101098291577,0.));
#20702=DIRECTION('',(0.475116216037135,-0.879923054169258,0.));
#20703=DIRECTION('center_axis',(0.,0.,1.));
#20704=DIRECTION('ref_axis',(1.,0.,0.));
#20705=DIRECTION('',(-0.87992305416926,0.475116216037131,0.));
#20706=DIRECTION('',(0.315101098291577,-0.949058110894924,0.));
#20707=DIRECTION('center_axis',(0.,0.,1.));
#20708=DIRECTION('ref_axis',(1.,0.,0.));
#20709=DIRECTION('',(-0.78405198070521,0.620695167978805,0.));
#20710=DIRECTION('',(0.145511793123284,-0.989356517167622,0.));
#20711=DIRECTION('center_axis',(0.,0.,1.));
#20712=DIRECTION('ref_axis',(1.,0.,0.));
#20713=DIRECTION('',(-0.66435788455688,0.747414611328349,0.));
#20714=DIRECTION('',(-0.028498814246539,-0.999593826304735,0.));
#20715=DIRECTION('center_axis',(0.,0.,1.));
#20716=DIRECTION('ref_axis',(1.,0.,0.));
#20717=DIRECTION('',(-0.524477610267605,0.851424239922721,0.));
#20718=DIRECTION('',(-0.201643499566573,-0.979458982848463,0.));
#20719=DIRECTION('center_axis',(0.,0.,1.));
#20720=DIRECTION('ref_axis',(1.,0.,0.));
#20721=DIRECTION('',(-0.368661349188821,0.929563773828498,0.));
#20722=DIRECTION('',(-0.368661349188821,-0.929563773828498,0.));
#20723=DIRECTION('center_axis',(0.,0.,1.));
#20724=DIRECTION('ref_axis',(1.,0.,0.));
#20725=DIRECTION('',(-0.201643499566578,0.979458982848462,0.));
#20726=DIRECTION('',(-0.524477610267605,-0.85142423992272,0.));
#20727=DIRECTION('center_axis',(0.,0.,1.));
#20728=DIRECTION('ref_axis',(1.,0.,0.));
#20729=DIRECTION('',(-0.0284988142465341,0.999593826304735,0.));
#20730=DIRECTION('',(-0.664357884556884,-0.747414611328346,0.));
#20731=DIRECTION('center_axis',(0.,0.,1.));
#20732=DIRECTION('ref_axis',(1.,0.,0.));
#20733=DIRECTION('',(0.145511793123284,0.989356517167622,0.));
#20734=DIRECTION('',(-0.78405198070521,-0.620695167978805,0.));
#20735=DIRECTION('center_axis',(0.,0.,1.));
#20736=DIRECTION('ref_axis',(1.,0.,0.));
#20737=DIRECTION('',(0.315101098291578,0.949058110894924,0.));
#20738=DIRECTION('',(-0.879923054169259,-0.475116216037132,0.));
#20739=DIRECTION('center_axis',(0.,0.,1.));
#20740=DIRECTION('ref_axis',(1.,0.,0.));
#20741=DIRECTION('',(0.475116216037133,0.879923054169259,0.));
#20742=DIRECTION('',(-0.949058110894923,-0.315101098291581,0.));
#20743=DIRECTION('center_axis',(0.,0.,1.));
#20744=DIRECTION('ref_axis',(1.,0.,0.));
#20745=DIRECTION('',(0.620695167978803,0.784051980705211,0.));
#20746=DIRECTION('',(-0.989356517167622,-0.145511793123284,0.));
#20747=DIRECTION('center_axis',(0.,0.,1.));
#20748=DIRECTION('ref_axis',(1.,0.,0.));
#20749=DIRECTION('',(0.747414611328348,0.664357884556882,0.));
#20750=DIRECTION('',(-0.999593826304735,0.0284988142465371,0.));
#20751=DIRECTION('center_axis',(0.,0.,1.));
#20752=DIRECTION('ref_axis',(1.,0.,0.));
#20753=DIRECTION('',(0.851424239922722,0.524477610267603,0.));
#20754=DIRECTION('',(-0.979458982848462,0.201643499566578,0.));
#20755=DIRECTION('center_axis',(0.,0.,1.));
#20756=DIRECTION('ref_axis',(1.,0.,0.));
#20757=DIRECTION('',(0.929563773828499,0.368661349188818,0.));
#20758=DIRECTION('',(-0.929563773828499,0.368661349188818,0.));
#20759=DIRECTION('center_axis',(0.,0.,1.));
#20760=DIRECTION('ref_axis',(1.,0.,0.));
#20761=DIRECTION('',(0.979458982848462,0.201643499566576,0.));
#20762=DIRECTION('',(-0.85142423992272,0.524477610267605,0.));
#20763=DIRECTION('center_axis',(0.,0.,1.));
#20764=DIRECTION('ref_axis',(1.,0.,0.));
#20765=DIRECTION('',(0.999593826304735,0.0284988142465395,0.));
#20766=DIRECTION('',(-0.747414611328348,0.664357884556882,0.));
#20767=DIRECTION('center_axis',(0.,0.,1.));
#20768=DIRECTION('ref_axis',(1.,0.,0.));
#20769=DIRECTION('',(0.989356517167621,-0.145511793123287,0.));
#20770=DIRECTION('',(-0.620695167978801,0.784051980705213,0.));
#20771=DIRECTION('center_axis',(0.,0.,1.));
#20772=DIRECTION('ref_axis',(1.,0.,0.));
#20773=DIRECTION('',(0.949058110894924,-0.315101098291577,0.));
#20774=DIRECTION('',(-0.475116216037132,0.879923054169259,0.));
#20775=DIRECTION('center_axis',(0.,0.,1.));
#20776=DIRECTION('ref_axis',(1.,0.,0.));
#20777=DIRECTION('',(0.879923054169259,-0.475116216037133,0.));
#20778=DIRECTION('',(-0.31510109829158,0.949058110894923,0.));
#20779=DIRECTION('center_axis',(0.,0.,1.));
#20780=DIRECTION('ref_axis',(1.,0.,0.));
#20781=DIRECTION('',(0.784051980705213,-0.620695167978802,0.));
#20782=DIRECTION('',(-0.145511793123287,0.989356517167621,0.));
#20783=DIRECTION('center_axis',(0.,0.,1.));
#20784=DIRECTION('ref_axis',(1.,0.,0.));
#20785=DIRECTION('',(0.664357884556883,-0.747414611328346,0.));
#20786=DIRECTION('',(0.028498814246538,0.999593826304735,0.));
#20787=DIRECTION('center_axis',(0.,0.,1.));
#20788=DIRECTION('ref_axis',(1.,0.,0.));
#20789=DIRECTION('',(0.524477610267604,-0.851424239922721,0.));
#20790=DIRECTION('',(0.201643499566577,0.979458982848462,0.));
#20791=DIRECTION('center_axis',(0.,0.,1.));
#20792=DIRECTION('ref_axis',(1.,0.,0.));
#20793=DIRECTION('',(0.368661349188819,-0.929563773828498,0.));
#20794=DIRECTION('',(0.368661349188819,0.929563773828498,0.));
#20795=DIRECTION('center_axis',(0.,0.,1.));
#20796=DIRECTION('ref_axis',(1.,0.,0.));
#20797=DIRECTION('',(0.201643499566577,-0.979458982848462,0.));
#20798=DIRECTION('',(0.524477610267603,0.851424239922722,0.));
#20799=DIRECTION('center_axis',(0.,0.,1.));
#20800=DIRECTION('ref_axis',(1.,0.,0.));
#20801=DIRECTION('',(0.0284988142465383,-0.999593826304735,0.));
#20802=DIRECTION('',(0.664357884556882,0.747414611328348,0.));
#20803=DIRECTION('center_axis',(0.,0.,1.));
#20804=DIRECTION('ref_axis',(1.,0.,0.));
#20805=DIRECTION('',(-0.145511793123286,-0.989356517167621,0.));
#20806=DIRECTION('',(0.784051980705211,0.620695167978803,0.));
#20807=DIRECTION('center_axis',(0.,0.,1.));
#20808=DIRECTION('ref_axis',(1.,0.,0.));
#20809=DIRECTION('',(-0.31510109829158,-0.949058110894923,0.));
#20810=DIRECTION('',(0.879923054169259,0.475116216037132,0.));
#20811=DIRECTION('center_axis',(0.,0.,1.));
#20812=DIRECTION('ref_axis',(1.,0.,0.));
#20813=DIRECTION('',(-0.475116216037132,-0.87992305416926,0.));
#20814=DIRECTION('',(0.949058110894923,0.31510109829158,0.));
#20815=DIRECTION('center_axis',(0.,0.,1.));
#20816=DIRECTION('ref_axis',(1.,0.,0.));
#20817=DIRECTION('',(-0.620695167978802,-0.784051980705212,0.));
#20818=DIRECTION('',(0.989356517167621,0.145511793123286,0.));
#20819=DIRECTION('center_axis',(0.,0.,1.));
#20820=DIRECTION('ref_axis',(1.,0.,0.));
#20821=DIRECTION('',(-0.747414611328347,-0.664357884556883,0.));
#20822=DIRECTION('',(0.999593826304735,-0.0284988142465376,0.));
#20823=DIRECTION('center_axis',(0.,0.,1.));
#20824=DIRECTION('ref_axis',(1.,0.,0.));
#20825=DIRECTION('',(-0.851424239922721,-0.524477610267604,0.));
#20826=DIRECTION('',(0.979458982848462,-0.201643499566577,0.));
#20827=DIRECTION('center_axis',(0.,0.,1.));
#20828=DIRECTION('ref_axis',(1.,0.,0.));
#20829=DIRECTION('',(-0.929563773828498,-0.368661349188819,0.));
#20830=DIRECTION('',(0.929563773828498,-0.368661349188819,0.));
#20831=DIRECTION('center_axis',(0.,0.,1.));
#20832=DIRECTION('ref_axis',(1.,0.,0.));
#20833=DIRECTION('',(-0.979458982848462,-0.201643499566578,0.));
#20834=DIRECTION('',(0.85142423992272,-0.524477610267605,0.));
#20835=DIRECTION('center_axis',(0.,0.,1.));
#20836=DIRECTION('ref_axis',(1.,0.,0.));
#20837=DIRECTION('center_axis',(0.,0.,1.));
#20838=DIRECTION('ref_axis',(1.,0.,0.));
#20839=DIRECTION('',(-1.,1.60246890531964E-16,0.));
#20840=DIRECTION('center_axis',(0.,0.,1.));
#20841=DIRECTION('ref_axis',(1.,0.,0.));
#20842=DIRECTION('center_axis',(0.,0.,1.));
#20843=DIRECTION('ref_axis',(1.,0.,0.));
#20844=DIRECTION('',(-0.5,0.866025403784439,0.));
#20845=DIRECTION('center_axis',(0.,0.,1.));
#20846=DIRECTION('ref_axis',(1.,0.,0.));
#20847=DIRECTION('center_axis',(0.,0.,1.));
#20848=DIRECTION('ref_axis',(1.,0.,0.));
#20849=DIRECTION('',(0.5,0.866025403784439,0.));
#20850=DIRECTION('center_axis',(0.,0.,1.));
#20851=DIRECTION('ref_axis',(1.,0.,0.));
#20852=DIRECTION('center_axis',(0.,0.,1.));
#20853=DIRECTION('ref_axis',(1.,0.,0.));
#20854=DIRECTION('',(1.,-1.60246890531964E-16,0.));
#20855=DIRECTION('center_axis',(0.,0.,1.));
#20856=DIRECTION('ref_axis',(1.,0.,0.));
#20857=DIRECTION('center_axis',(0.,0.,1.));
#20858=DIRECTION('ref_axis',(1.,0.,0.));
#20859=DIRECTION('',(0.5,-0.866025403784439,0.));
#20860=DIRECTION('center_axis',(0.,0.,1.));
#20861=DIRECTION('ref_axis',(1.,0.,0.));
#20862=DIRECTION('center_axis',(0.,0.,1.));
#20863=DIRECTION('ref_axis',(1.,0.,0.));
#20864=DIRECTION('',(-0.5,-0.866025403784439,0.));
#20865=DIRECTION('center_axis',(0.,0.,1.));
#20866=DIRECTION('ref_axis',(1.,0.,0.));
#20867=DIRECTION('center_axis',(0.,0.,1.));
#20868=DIRECTION('ref_axis',(1.,0.,0.));
#20869=DIRECTION('',(-0.85530665792059,-1.04744856091187E-16,0.518122110044255));
#20870=DIRECTION('center_axis',(0.,0.,-1.));
#20871=DIRECTION('ref_axis',(1.,0.,0.));
#20872=DIRECTION('center_axis',(0.,0.,-1.));
#20873=DIRECTION('ref_axis',(1.,0.,0.));
#20874=DIRECTION('center_axis',(0.,0.,-1.));
#20875=DIRECTION('ref_axis',(1.,0.,0.));
#20876=DIRECTION('center_axis',(0.,0.,-1.));
#20877=DIRECTION('ref_axis',(1.,0.,0.));
#20878=DIRECTION('center_axis',(0.,0.,-1.));
#20879=DIRECTION('ref_axis',(1.,0.,0.));
#20880=DIRECTION('center_axis',(0.,0.,-1.));
#20881=DIRECTION('ref_axis',(1.,0.,0.));
#20882=DIRECTION('center_axis',(0.,0.,-1.));
#20883=DIRECTION('ref_axis',(1.,0.,0.));
#20884=DIRECTION('center_axis',(-0.866025403784439,0.5,0.));
#20885=DIRECTION('ref_axis',(0.5,0.866025403784439,0.));
#20886=DIRECTION('',(0.,0.,-1.));
#20887=DIRECTION('',(0.5,0.866025403784439,0.));
#20888=DIRECTION('',(0.,0.,-1.));
#20889=DIRECTION('center_axis',(-0.866025403784439,0.5,0.));
#20890=DIRECTION('ref_axis',(0.5,0.866025403784439,0.));
#20891=DIRECTION('',(0.,0.,-1.));
#20892=DIRECTION('',(0.5,0.866025403784439,0.));
#20893=DIRECTION('center_axis',(1.60246890531964E-16,1.,0.));
#20894=DIRECTION('ref_axis',(1.,-1.60246890531964E-16,0.));
#20895=DIRECTION('',(0.,0.,-1.));
#20896=DIRECTION('',(1.,-1.60246890531964E-16,0.));
#20897=DIRECTION('center_axis',(1.60246890531964E-16,1.,0.));
#20898=DIRECTION('ref_axis',(1.,-1.60246890531964E-16,0.));
#20899=DIRECTION('',(1.,-1.60246890531964E-16,0.));
#20900=DIRECTION('',(0.,0.,-1.));
#20901=DIRECTION('center_axis',(1.60246890531964E-16,1.,0.));
#20902=DIRECTION('ref_axis',(1.,-1.60246890531964E-16,0.));
#20903=DIRECTION('',(0.,0.,-1.));
#20904=DIRECTION('',(1.,-1.60246890531964E-16,0.));
#20905=DIRECTION('center_axis',(-0.866025403784439,-0.5,0.));
#20906=DIRECTION('ref_axis',(-0.5,0.866025403784439,0.));
#20907=DIRECTION('',(-0.5,0.866025403784439,0.));
#20908=DIRECTION('',(0.,0.,-1.));
#20909=DIRECTION('center_axis',(-0.866025403784439,-0.5,0.));
#20910=DIRECTION('ref_axis',(-0.5,0.866025403784439,0.));
#20911=DIRECTION('',(0.,0.,-1.));
#20912=DIRECTION('',(-0.5,0.866025403784439,0.));
#20913=DIRECTION('center_axis',(0.866025403784439,0.5,0.));
#20914=DIRECTION('ref_axis',(0.5,-0.866025403784439,0.));
#20915=DIRECTION('',(0.,0.,-1.));
#20916=DIRECTION('',(0.5,-0.866025403784439,0.));
#20917=DIRECTION('center_axis',(0.866025403784439,0.5,0.));
#20918=DIRECTION('ref_axis',(0.5,-0.866025403784439,0.));
#20919=DIRECTION('',(0.5,-0.866025403784439,0.));
#20920=DIRECTION('',(0.,0.,-1.));
#20921=DIRECTION('center_axis',(0.866025403784439,0.5,0.));
#20922=DIRECTION('ref_axis',(0.5,-0.866025403784439,0.));
#20923=DIRECTION('',(0.5,-0.866025403784439,0.));
#20924=DIRECTION('center_axis',(0.,0.,-1.));
#20925=DIRECTION('ref_axis',(-1.,0.,0.));
#20926=DIRECTION('',(0.5,0.866025403784439,0.));
#20927=DIRECTION('center_axis',(0.,0.,-1.));
#20928=DIRECTION('ref_axis',(-1.,0.,0.));
#20929=DIRECTION('center_axis',(0.,0.,-1.));
#20930=DIRECTION('ref_axis',(-1.,0.,0.));
#20931=DIRECTION('',(-0.5,-0.866025403784439,0.));
#20932=DIRECTION('center_axis',(0.,0.,-1.));
#20933=DIRECTION('ref_axis',(-1.,0.,0.));
#20934=DIRECTION('',(-1.,1.60246890531964E-16,0.));
#20935=DIRECTION('',(-0.5,-0.866025403784439,0.));
#20936=DIRECTION('center_axis',(0.,0.,-1.));
#20937=DIRECTION('ref_axis',(-1.,0.,0.));
#20938=DIRECTION('',(-1.,1.60246890531964E-16,0.));
#20939=DIRECTION('center_axis',(0.,0.,-1.));
#20940=DIRECTION('ref_axis',(-1.,0.,0.));
#20941=DIRECTION('',(-0.5,0.866025403784439,0.));
#20942=DIRECTION('center_axis',(0.866025403784439,-0.5,0.));
#20943=DIRECTION('ref_axis',(-0.5,-0.866025403784439,0.));
#20944=DIRECTION('',(0.,0.,-1.));
#20945=DIRECTION('',(-0.5,-0.866025403784439,0.));
#20946=DIRECTION('center_axis',(0.866025403784439,-0.5,0.));
#20947=DIRECTION('ref_axis',(-0.5,-0.866025403784439,0.));
#20948=DIRECTION('',(0.,0.,-1.));
#20949=DIRECTION('center_axis',(0.866025403784439,-0.5,0.));
#20950=DIRECTION('ref_axis',(-0.5,-0.866025403784439,0.));
#20951=DIRECTION('center_axis',(-1.60246890531964E-16,-1.,0.));
#20952=DIRECTION('ref_axis',(-1.,1.60246890531964E-16,0.));
#20953=DIRECTION('center_axis',(-1.60246890531964E-16,-1.,0.));
#20954=DIRECTION('ref_axis',(-1.,1.60246890531964E-16,0.));
#20955=DIRECTION('',(-1.,1.60246890531964E-16,0.));
#20956=DIRECTION('center_axis',(-0.866025403784439,0.5,0.));
#20957=DIRECTION('ref_axis',(0.5,0.866025403784439,0.));
#20958=DIRECTION('center_axis',(-0.866025403784439,-0.5,0.));
#20959=DIRECTION('ref_axis',(-0.5,0.866025403784439,0.));
#20960=DIRECTION('center_axis',(-1.60246890531964E-16,-1.,0.));
#20961=DIRECTION('ref_axis',(-1.,1.60246890531964E-16,0.));
#20962=DIRECTION('center_axis',(-0.0284988142465338,0.999593826304735,0.));
#20963=DIRECTION('ref_axis',(0.999593826304735,0.0284988142465338,0.));
#20964=DIRECTION('',(0.,0.,-1.));
#20965=DIRECTION('',(0.,0.,-1.));
#20966=DIRECTION('center_axis',(-0.664357884556884,-0.747414611328346,0.));
#20967=DIRECTION('ref_axis',(-0.747414611328346,0.664357884556884,0.));
#20968=DIRECTION('',(0.,0.,1.));
#20969=DIRECTION('center_axis',(0.315101098291577,0.949058110894924,0.));
#20970=DIRECTION('ref_axis',(0.949058110894924,-0.315101098291577,0.));
#20971=DIRECTION('',(0.,0.,-1.));
#20972=DIRECTION('',(0.,0.,-1.));
#20973=DIRECTION('center_axis',(-0.879923054169258,-0.475116216037135,0.));
#20974=DIRECTION('ref_axis',(-0.475116216037135,0.879923054169258,0.));
#20975=DIRECTION('',(0.,0.,1.));
#20976=DIRECTION('center_axis',(0.620695167978805,0.78405198070521,0.));
#20977=DIRECTION('ref_axis',(0.78405198070521,-0.620695167978805,0.));
#20978=DIRECTION('',(0.,0.,-1.));
#20979=DIRECTION('',(0.,0.,-1.));
#20980=DIRECTION('center_axis',(-0.989356517167622,-0.145511793123284,0.));
#20981=DIRECTION('ref_axis',(-0.145511793123284,0.989356517167622,0.));
#20982=DIRECTION('',(0.,0.,1.));
#20983=DIRECTION('center_axis',(0.851424239922721,0.524477610267605,0.));
#20984=DIRECTION('ref_axis',(0.524477610267605,-0.851424239922721,0.));
#20985=DIRECTION('',(0.,0.,-1.));
#20986=DIRECTION('',(0.,0.,-1.));
#20987=DIRECTION('center_axis',(-0.979458982848463,0.201643499566573,0.));
#20988=DIRECTION('ref_axis',(0.201643499566573,0.979458982848463,0.));
#20989=DIRECTION('',(0.,0.,1.));
#20990=DIRECTION('center_axis',(0.979458982848462,0.201643499566578,0.));
#20991=DIRECTION('ref_axis',(0.201643499566578,-0.979458982848462,0.));
#20992=DIRECTION('',(0.,0.,-1.));
#20993=DIRECTION('',(0.,0.,-1.));
#20994=DIRECTION('center_axis',(-0.85142423992272,0.524477610267605,0.));
#20995=DIRECTION('ref_axis',(0.524477610267605,0.85142423992272,0.));
#20996=DIRECTION('',(0.,0.,1.));
#20997=DIRECTION('center_axis',(0.989356517167622,-0.145511793123284,0.));
#20998=DIRECTION('ref_axis',(-0.145511793123284,-0.989356517167622,0.));
#20999=DIRECTION('',(0.,0.,-1.));
#21000=DIRECTION('',(0.,0.,-1.));
#21001=DIRECTION('center_axis',(-0.620695167978805,0.78405198070521,0.));
#21002=DIRECTION('ref_axis',(0.78405198070521,0.620695167978805,0.));
#21003=DIRECTION('',(0.,0.,1.));
#21004=DIRECTION('center_axis',(0.879923054169259,-0.475116216037133,0.));
#21005=DIRECTION('ref_axis',(-0.475116216037133,-0.879923054169259,0.));
#21006=DIRECTION('',(0.,0.,-1.));
#21007=DIRECTION('',(0.,0.,-1.));
#21008=DIRECTION('center_axis',(-0.315101098291581,0.949058110894923,0.));
#21009=DIRECTION('ref_axis',(0.949058110894923,0.315101098291581,0.));
#21010=DIRECTION('',(0.,0.,1.));
#21011=DIRECTION('center_axis',(0.664357884556882,-0.747414611328348,0.));
#21012=DIRECTION('ref_axis',(-0.747414611328348,-0.664357884556882,0.));
#21013=DIRECTION('',(0.,0.,-1.));
#21014=DIRECTION('',(0.,0.,-1.));
#21015=DIRECTION('center_axis',(0.0284988142465371,0.999593826304735,0.));
#21016=DIRECTION('ref_axis',(0.999593826304735,-0.0284988142465371,0.));
#21017=DIRECTION('',(0.,0.,1.));
#21018=DIRECTION('center_axis',(0.368661349188818,-0.929563773828499,0.));
#21019=DIRECTION('ref_axis',(-0.929563773828499,-0.368661349188818,0.));
#21020=DIRECTION('',(0.,0.,-1.));
#21021=DIRECTION('',(0.,0.,-1.));
#21022=DIRECTION('center_axis',(0.368661349188818,0.929563773828499,0.));
#21023=DIRECTION('ref_axis',(0.929563773828499,-0.368661349188818,0.));
#21024=DIRECTION('',(0.,0.,1.));
#21025=DIRECTION('center_axis',(0.201643499566576,-0.979458982848462,0.));
#21026=DIRECTION('ref_axis',(-0.979458982848462,-0.201643499566576,0.));
#21027=DIRECTION('',(0.,0.,-1.));
#21028=DIRECTION('',(0.,0.,-1.));
#21029=DIRECTION('center_axis',(0.524477610267605,0.85142423992272,0.));
#21030=DIRECTION('ref_axis',(0.85142423992272,-0.524477610267605,0.));
#21031=DIRECTION('',(0.,0.,1.));
#21032=DIRECTION('center_axis',(-0.145511793123287,-0.989356517167621,0.));
#21033=DIRECTION('ref_axis',(-0.989356517167621,0.145511793123287,0.));
#21034=DIRECTION('',(0.,0.,-1.));
#21035=DIRECTION('',(0.,0.,-1.));
#21036=DIRECTION('center_axis',(0.784051980705213,0.620695167978801,0.));
#21037=DIRECTION('ref_axis',(0.620695167978801,-0.784051980705213,0.));
#21038=DIRECTION('',(0.,0.,1.));
#21039=DIRECTION('center_axis',(-0.475116216037133,-0.879923054169259,0.));
#21040=DIRECTION('ref_axis',(-0.879923054169259,0.475116216037133,0.));
#21041=DIRECTION('',(0.,0.,-1.));
#21042=DIRECTION('',(0.,0.,-1.));
#21043=DIRECTION('center_axis',(0.949058110894923,0.31510109829158,0.));
#21044=DIRECTION('ref_axis',(0.31510109829158,-0.949058110894923,0.));
#21045=DIRECTION('',(0.,0.,1.));
#21046=DIRECTION('center_axis',(-0.747414611328346,-0.664357884556883,0.));
#21047=DIRECTION('ref_axis',(-0.664357884556883,0.747414611328346,0.));
#21048=DIRECTION('',(0.,0.,-1.));
#21049=DIRECTION('',(0.,0.,-1.));
#21050=DIRECTION('center_axis',(0.999593826304735,-0.028498814246538,0.));
#21051=DIRECTION('ref_axis',(-0.028498814246538,-0.999593826304735,0.));
#21052=DIRECTION('',(0.,0.,1.));
#21053=DIRECTION('center_axis',(-0.929563773828498,-0.368661349188819,0.));
#21054=DIRECTION('ref_axis',(-0.368661349188819,0.929563773828498,0.));
#21055=DIRECTION('',(0.,0.,-1.));
#21056=DIRECTION('',(0.,0.,-1.));
#21057=DIRECTION('center_axis',(0.929563773828498,-0.368661349188819,0.));
#21058=DIRECTION('ref_axis',(-0.368661349188819,-0.929563773828498,0.));
#21059=DIRECTION('',(0.,0.,1.));
#21060=DIRECTION('center_axis',(-0.999593826304735,-0.0284988142465383,
0.));
#21061=DIRECTION('ref_axis',(-0.0284988142465383,0.999593826304735,0.));
#21062=DIRECTION('',(0.,0.,-1.));
#21063=DIRECTION('',(0.,0.,-1.));
#21064=DIRECTION('center_axis',(0.747414611328348,-0.664357884556882,0.));
#21065=DIRECTION('ref_axis',(-0.664357884556882,-0.747414611328348,0.));
#21066=DIRECTION('',(0.,0.,1.));
#21067=DIRECTION('center_axis',(-0.949058110894923,0.31510109829158,0.));
#21068=DIRECTION('ref_axis',(0.31510109829158,0.949058110894923,0.));
#21069=DIRECTION('',(0.,0.,-1.));
#21070=DIRECTION('',(0.,0.,-1.));
#21071=DIRECTION('center_axis',(0.475116216037132,-0.879923054169259,0.));
#21072=DIRECTION('ref_axis',(-0.879923054169259,-0.475116216037132,0.));
#21073=DIRECTION('',(0.,0.,1.));
#21074=DIRECTION('center_axis',(-0.784051980705212,0.620695167978802,0.));
#21075=DIRECTION('ref_axis',(0.620695167978802,0.784051980705212,0.));
#21076=DIRECTION('',(0.,0.,-1.));
#21077=DIRECTION('',(0.,0.,-1.));
#21078=DIRECTION('center_axis',(0.145511793123286,-0.989356517167621,0.));
#21079=DIRECTION('ref_axis',(-0.989356517167621,-0.145511793123286,0.));
#21080=DIRECTION('',(0.,0.,1.));
#21081=DIRECTION('center_axis',(-0.524477610267604,0.851424239922721,0.));
#21082=DIRECTION('ref_axis',(0.851424239922721,0.524477610267604,0.));
#21083=DIRECTION('',(0.,0.,-1.));
#21084=DIRECTION('',(0.,0.,-1.));
#21085=DIRECTION('center_axis',(-0.201643499566577,-0.979458982848462,0.));
#21086=DIRECTION('ref_axis',(-0.979458982848462,0.201643499566577,0.));
#21087=DIRECTION('',(0.,0.,1.));
#21088=DIRECTION('center_axis',(-0.664357884556883,0.747414611328347,0.));
#21089=DIRECTION('ref_axis',(0.747414611328347,0.664357884556883,0.));
#21090=DIRECTION('',(0.,0.,-1.));
#21091=DIRECTION('',(0.,0.,-1.));
#21092=DIRECTION('center_axis',(-0.0284988142465376,-0.999593826304735,
0.));
#21093=DIRECTION('ref_axis',(-0.999593826304735,0.0284988142465376,0.));
#21094=DIRECTION('',(0.,0.,1.));
#21095=DIRECTION('center_axis',(-0.87992305416926,0.475116216037132,0.));
#21096=DIRECTION('ref_axis',(0.475116216037132,0.87992305416926,0.));
#21097=DIRECTION('',(0.,0.,-1.));
#21098=DIRECTION('',(0.,0.,-1.));
#21099=DIRECTION('center_axis',(0.31510109829158,-0.949058110894923,0.));
#21100=DIRECTION('ref_axis',(-0.949058110894923,-0.31510109829158,0.));
#21101=DIRECTION('',(0.,0.,1.));
#21102=DIRECTION('center_axis',(-0.989356517167621,0.145511793123286,0.));
#21103=DIRECTION('ref_axis',(0.145511793123286,0.989356517167621,0.));
#21104=DIRECTION('',(0.,0.,-1.));
#21105=DIRECTION('',(0.,0.,-1.));
#21106=DIRECTION('center_axis',(0.620695167978803,-0.784051980705211,0.));
#21107=DIRECTION('ref_axis',(-0.784051980705211,-0.620695167978803,0.));
#21108=DIRECTION('',(0.,0.,1.));
#21109=DIRECTION('center_axis',(-0.979458982848462,-0.201643499566577,0.));
#21110=DIRECTION('ref_axis',(-0.201643499566577,0.979458982848462,0.));
#21111=DIRECTION('',(0.,0.,-1.));
#21112=DIRECTION('',(0.,0.,-1.));
#21113=DIRECTION('center_axis',(0.851424239922722,-0.524477610267603,0.));
#21114=DIRECTION('ref_axis',(-0.524477610267603,-0.851424239922722,0.));
#21115=DIRECTION('',(0.,0.,1.));
#21116=DIRECTION('center_axis',(-0.851424239922721,-0.524477610267604,0.));
#21117=DIRECTION('ref_axis',(-0.524477610267604,0.851424239922721,0.));
#21118=DIRECTION('',(0.,0.,-1.));
#21119=DIRECTION('',(0.,0.,-1.));
#21120=DIRECTION('center_axis',(0.979458982848462,-0.201643499566577,0.));
#21121=DIRECTION('ref_axis',(-0.201643499566577,-0.979458982848462,0.));
#21122=DIRECTION('',(0.,0.,1.));
#21123=DIRECTION('center_axis',(-0.620695167978802,-0.784051980705213,0.));
#21124=DIRECTION('ref_axis',(-0.784051980705213,0.620695167978802,0.));
#21125=DIRECTION('',(0.,0.,-1.));
#21126=DIRECTION('',(0.,0.,-1.));
#21127=DIRECTION('center_axis',(0.989356517167621,0.145511793123287,0.));
#21128=DIRECTION('ref_axis',(0.145511793123287,-0.989356517167621,0.));
#21129=DIRECTION('',(0.,0.,1.));
#21130=DIRECTION('center_axis',(-0.315101098291577,-0.949058110894924,0.));
#21131=DIRECTION('ref_axis',(-0.949058110894924,0.315101098291577,0.));
#21132=DIRECTION('',(0.,0.,-1.));
#21133=DIRECTION('',(0.,0.,-1.));
#21134=DIRECTION('center_axis',(0.879923054169259,0.475116216037132,0.));
#21135=DIRECTION('ref_axis',(0.475116216037132,-0.879923054169259,0.));
#21136=DIRECTION('',(0.,0.,1.));
#21137=DIRECTION('center_axis',(0.0284988142465395,-0.999593826304735,0.));
#21138=DIRECTION('ref_axis',(-0.999593826304735,-0.0284988142465395,0.));
#21139=DIRECTION('',(0.,0.,-1.));
#21140=DIRECTION('',(0.,0.,-1.));
#21141=DIRECTION('center_axis',(0.664357884556882,0.747414611328348,0.));
#21142=DIRECTION('ref_axis',(0.747414611328348,-0.664357884556882,0.));
#21143=DIRECTION('',(0.,0.,1.));
#21144=DIRECTION('center_axis',(-0.368661349188819,0.929563773828498,0.));
#21145=DIRECTION('ref_axis',(0.929563773828498,0.368661349188819,0.));
#21146=DIRECTION('',(0.,0.,-1.));
#21147=DIRECTION('',(0.,0.,-1.));
#21148=DIRECTION('center_axis',(-0.368661349188819,-0.929563773828498,0.));
#21149=DIRECTION('ref_axis',(-0.929563773828498,0.368661349188819,0.));
#21150=DIRECTION('',(0.,0.,1.));
#21151=DIRECTION('center_axis',(0.524477610267603,-0.851424239922722,0.));
#21152=DIRECTION('ref_axis',(-0.851424239922722,-0.524477610267603,0.));
#21153=DIRECTION('',(0.,0.,-1.));
#21154=DIRECTION('',(0.,0.,-1.));
#21155=DIRECTION('center_axis',(0.201643499566578,0.979458982848462,0.));
#21156=DIRECTION('ref_axis',(0.979458982848462,-0.201643499566578,0.));
#21157=DIRECTION('',(0.,0.,1.));
#21158=DIRECTION('center_axis',(0.784051980705211,-0.620695167978803,0.));
#21159=DIRECTION('ref_axis',(-0.620695167978803,-0.784051980705211,0.));
#21160=DIRECTION('',(0.,0.,-1.));
#21161=DIRECTION('',(0.,0.,-1.));
#21162=DIRECTION('center_axis',(-0.145511793123284,0.989356517167622,0.));
#21163=DIRECTION('ref_axis',(0.989356517167622,0.145511793123284,0.));
#21164=DIRECTION('',(0.,0.,1.));
#21165=DIRECTION('center_axis',(0.949058110894924,-0.315101098291578,0.));
#21166=DIRECTION('ref_axis',(-0.315101098291578,-0.949058110894924,0.));
#21167=DIRECTION('',(0.,0.,-1.));
#21168=DIRECTION('',(0.,0.,-1.));
#21169=DIRECTION('center_axis',(-0.475116216037132,0.879923054169259,0.));
#21170=DIRECTION('ref_axis',(0.879923054169259,0.475116216037132,0.));
#21171=DIRECTION('',(0.,0.,1.));
#21172=DIRECTION('center_axis',(0.999593826304735,0.0284988142465341,0.));
#21173=DIRECTION('ref_axis',(0.0284988142465341,-0.999593826304735,0.));
#21174=DIRECTION('',(0.,0.,-1.));
#21175=DIRECTION('',(0.,0.,-1.));
#21176=DIRECTION('center_axis',(-0.747414611328346,0.664357884556884,0.));
#21177=DIRECTION('ref_axis',(0.664357884556884,0.747414611328346,0.));
#21178=DIRECTION('',(0.,0.,1.));
#21179=DIRECTION('center_axis',(0.929563773828498,0.368661349188821,0.));
#21180=DIRECTION('ref_axis',(0.368661349188821,-0.929563773828498,0.));
#21181=DIRECTION('',(0.,0.,-1.));
#21182=DIRECTION('',(0.,0.,-1.));
#21183=DIRECTION('center_axis',(-0.929563773828498,0.368661349188821,0.));
#21184=DIRECTION('ref_axis',(0.368661349188821,0.929563773828498,0.));
#21185=DIRECTION('',(0.,0.,1.));
#21186=DIRECTION('center_axis',(0.747414611328349,0.66435788455688,0.));
#21187=DIRECTION('ref_axis',(0.66435788455688,-0.747414611328349,0.));
#21188=DIRECTION('',(0.,0.,-1.));
#21189=DIRECTION('',(0.,0.,-1.));
#21190=DIRECTION('center_axis',(-0.999593826304735,0.028498814246539,0.));
#21191=DIRECTION('ref_axis',(0.028498814246539,0.999593826304735,0.));
#21192=DIRECTION('',(0.,0.,1.));
#21193=DIRECTION('center_axis',(0.475116216037131,0.87992305416926,0.));
#21194=DIRECTION('ref_axis',(0.87992305416926,-0.475116216037131,0.));
#21195=DIRECTION('',(0.,0.,-1.));
#21196=DIRECTION('',(0.,0.,-1.));
#21197=DIRECTION('center_axis',(-0.949058110894924,-0.315101098291577,0.));
#21198=DIRECTION('ref_axis',(-0.315101098291577,0.949058110894924,0.));
#21199=DIRECTION('',(0.,0.,1.));
#21200=DIRECTION('center_axis',(0.145511793123284,0.989356517167622,0.));
#21201=DIRECTION('ref_axis',(0.989356517167622,-0.145511793123284,0.));
#21202=DIRECTION('',(0.,0.,-1.));
#21203=DIRECTION('',(0.,0.,-1.));
#21204=DIRECTION('center_axis',(-0.78405198070521,-0.620695167978805,0.));
#21205=DIRECTION('ref_axis',(-0.620695167978805,0.78405198070521,0.));
#21206=DIRECTION('',(0.,0.,1.));
#21207=DIRECTION('center_axis',(-0.201643499566578,0.979458982848462,0.));
#21208=DIRECTION('ref_axis',(0.979458982848462,0.201643499566578,0.));
#21209=DIRECTION('',(0.,0.,-1.));
#21210=DIRECTION('',(0.,0.,-1.));
#21211=DIRECTION('center_axis',(-0.524477610267605,-0.85142423992272,0.));
#21212=DIRECTION('ref_axis',(-0.85142423992272,0.524477610267605,0.));
#21213=DIRECTION('',(0.,0.,1.));
#21214=DIRECTION('center_axis',(0.,0.,1.));
#21215=DIRECTION('ref_axis',(1.,0.,0.));
#21216=DIRECTION('center_axis',(0.,0.,1.));
#21217=DIRECTION('ref_axis',(1.,0.,0.));
#21218=DIRECTION('center_axis',(0.,0.,1.));
#21219=DIRECTION('ref_axis',(1.,0.,0.));
#21220=DIRECTION('center_axis',(0.,0.,1.));
#21221=DIRECTION('ref_axis',(1.,0.,0.));
#21222=DIRECTION('center_axis',(0.,0.,1.));
#21223=DIRECTION('ref_axis',(1.,0.,0.));
#21224=DIRECTION('center_axis',(0.,0.,1.));
#21225=DIRECTION('ref_axis',(1.,0.,0.));
#21226=DIRECTION('center_axis',(0.,0.,1.));
#21227=DIRECTION('ref_axis',(1.,0.,0.));
#21228=DIRECTION('center_axis',(0.,0.,1.));
#21229=DIRECTION('ref_axis',(1.,0.,0.));
#21230=DIRECTION('center_axis',(0.,0.,1.));
#21231=DIRECTION('ref_axis',(1.,0.,0.));
#21232=DIRECTION('center_axis',(0.,0.,1.));
#21233=DIRECTION('ref_axis',(1.,0.,0.));
#21234=DIRECTION('center_axis',(0.,0.,1.));
#21235=DIRECTION('ref_axis',(1.,0.,0.));
#21236=DIRECTION('center_axis',(0.,0.,1.));
#21237=DIRECTION('ref_axis',(1.,0.,0.));
#21238=DIRECTION('center_axis',(0.,0.,1.));
#21239=DIRECTION('ref_axis',(1.,0.,0.));
#21240=DIRECTION('center_axis',(0.,0.,1.));
#21241=DIRECTION('ref_axis',(1.,0.,0.));
#21242=DIRECTION('center_axis',(0.,0.,1.));
#21243=DIRECTION('ref_axis',(1.,0.,0.));
#21244=DIRECTION('center_axis',(0.,0.,1.));
#21245=DIRECTION('ref_axis',(1.,0.,0.));
#21246=DIRECTION('center_axis',(0.,0.,1.));
#21247=DIRECTION('ref_axis',(1.,0.,0.));
#21248=DIRECTION('center_axis',(0.,0.,1.));
#21249=DIRECTION('ref_axis',(1.,0.,0.));
#21250=DIRECTION('center_axis',(0.,0.,1.));
#21251=DIRECTION('ref_axis',(1.,0.,0.));
#21252=DIRECTION('center_axis',(0.,0.,1.));
#21253=DIRECTION('ref_axis',(1.,0.,0.));
#21254=DIRECTION('center_axis',(0.,0.,1.));
#21255=DIRECTION('ref_axis',(1.,0.,0.));
#21256=DIRECTION('center_axis',(0.,0.,1.));
#21257=DIRECTION('ref_axis',(1.,0.,0.));
#21258=DIRECTION('center_axis',(0.,0.,1.));
#21259=DIRECTION('ref_axis',(1.,0.,0.));
#21260=DIRECTION('center_axis',(0.,0.,1.));
#21261=DIRECTION('ref_axis',(1.,0.,0.));
#21262=DIRECTION('center_axis',(0.,0.,1.));
#21263=DIRECTION('ref_axis',(1.,0.,0.));
#21264=DIRECTION('center_axis',(0.,0.,1.));
#21265=DIRECTION('ref_axis',(1.,0.,0.));
#21266=DIRECTION('center_axis',(0.,0.,1.));
#21267=DIRECTION('ref_axis',(1.,0.,0.));
#21268=DIRECTION('center_axis',(0.,0.,1.));
#21269=DIRECTION('ref_axis',(1.,0.,0.));
#21270=DIRECTION('center_axis',(0.,0.,1.));
#21271=DIRECTION('ref_axis',(1.,0.,0.));
#21272=DIRECTION('center_axis',(0.,0.,1.));
#21273=DIRECTION('ref_axis',(1.,0.,0.));
#21274=DIRECTION('center_axis',(0.,0.,1.));
#21275=DIRECTION('ref_axis',(1.,0.,0.));
#21276=DIRECTION('center_axis',(0.,0.,1.));
#21277=DIRECTION('ref_axis',(1.,0.,0.));
#21278=DIRECTION('center_axis',(0.,0.,1.));
#21279=DIRECTION('ref_axis',(1.,0.,0.));
#21280=DIRECTION('center_axis',(0.,0.,1.));
#21281=DIRECTION('ref_axis',(1.,0.,0.));
#21282=DIRECTION('center_axis',(0.,0.,1.));
#21283=DIRECTION('ref_axis',(1.,0.,0.));
#21284=DIRECTION('center_axis',(0.,0.,1.));
#21285=DIRECTION('ref_axis',(1.,0.,0.));
#21286=DIRECTION('center_axis',(0.,0.,1.));
#21287=DIRECTION('ref_axis',(1.,0.,0.));
#21288=DIRECTION('center_axis',(0.,0.,1.));
#21289=DIRECTION('ref_axis',(1.,0.,0.));
#21290=DIRECTION('center_axis',(0.,0.,1.));
#21291=DIRECTION('ref_axis',(1.,0.,0.));
#21292=DIRECTION('center_axis',(0.,0.,1.));
#21293=DIRECTION('ref_axis',(1.,0.,0.));
#21294=DIRECTION('center_axis',(0.,0.,1.));
#21295=DIRECTION('ref_axis',(1.,0.,0.));
#21296=DIRECTION('center_axis',(0.,0.,1.));
#21297=DIRECTION('ref_axis',(1.,0.,0.));
#21298=DIRECTION('center_axis',(0.,0.,1.));
#21299=DIRECTION('ref_axis',(1.,0.,0.));
#21300=DIRECTION('center_axis',(0.,0.,1.));
#21301=DIRECTION('ref_axis',(1.,0.,0.));
#21302=DIRECTION('center_axis',(0.,0.,1.));
#21303=DIRECTION('ref_axis',(1.,0.,0.));
#21304=DIRECTION('center_axis',(0.,0.,1.));
#21305=DIRECTION('ref_axis',(1.,0.,0.));
#21306=DIRECTION('center_axis',(0.,0.,1.));
#21307=DIRECTION('ref_axis',(1.,0.,0.));
#21308=DIRECTION('center_axis',(0.,0.,1.));
#21309=DIRECTION('ref_axis',(1.,0.,0.));
#21310=DIRECTION('center_axis',(0.,0.,1.));
#21311=DIRECTION('ref_axis',(1.,0.,0.));
#21312=DIRECTION('center_axis',(0.,0.,1.));
#21313=DIRECTION('ref_axis',(1.,0.,0.));
#21314=DIRECTION('center_axis',(0.,0.,1.));
#21315=DIRECTION('ref_axis',(1.,0.,0.));
#21316=DIRECTION('center_axis',(0.,0.,1.));
#21317=DIRECTION('ref_axis',(1.,0.,0.));
#21318=DIRECTION('center_axis',(0.,0.,1.));
#21319=DIRECTION('ref_axis',(1.,0.,0.));
#21320=DIRECTION('center_axis',(0.,0.,1.));
#21321=DIRECTION('ref_axis',(1.,0.,0.));
#21322=DIRECTION('center_axis',(0.,0.,1.));
#21323=DIRECTION('ref_axis',(1.,0.,0.));
#21324=DIRECTION('center_axis',(0.,0.,1.));
#21325=DIRECTION('ref_axis',(1.,0.,0.));
#21326=DIRECTION('center_axis',(0.,0.,1.));
#21327=DIRECTION('ref_axis',(1.,0.,0.));
#21328=DIRECTION('center_axis',(0.,0.,1.));
#21329=DIRECTION('ref_axis',(1.,0.,0.));
#21330=DIRECTION('center_axis',(0.,0.,1.));
#21331=DIRECTION('ref_axis',(1.,0.,0.));
#21332=DIRECTION('center_axis',(0.,0.,1.));
#21333=DIRECTION('ref_axis',(1.,0.,0.));
#21334=DIRECTION('center_axis',(0.,0.,1.));
#21335=DIRECTION('ref_axis',(1.,0.,0.));
#21336=DIRECTION('center_axis',(0.,0.,1.));
#21337=DIRECTION('ref_axis',(1.,0.,0.));
#21338=DIRECTION('center_axis',(0.,0.,1.));
#21339=DIRECTION('ref_axis',(1.,0.,0.));
#21340=DIRECTION('center_axis',(0.,0.,1.));
#21341=DIRECTION('ref_axis',(1.,0.,0.));
#21342=DIRECTION('center_axis',(0.,0.,1.));
#21343=DIRECTION('ref_axis',(1.,0.,0.));
#21344=DIRECTION('center_axis',(0.,0.,1.));
#21345=DIRECTION('ref_axis',(1.,0.,0.));
#21346=DIRECTION('center_axis',(0.,0.,1.));
#21347=DIRECTION('ref_axis',(1.,0.,0.));
#21348=DIRECTION('center_axis',(0.,0.,1.));
#21349=DIRECTION('ref_axis',(1.,0.,0.));
#21350=DIRECTION('center_axis',(0.,0.,1.));
#21351=DIRECTION('ref_axis',(1.,0.,0.));
#21352=DIRECTION('center_axis',(0.,0.,1.));
#21353=DIRECTION('ref_axis',(1.,0.,0.));
#21354=DIRECTION('center_axis',(0.,0.,1.));
#21355=DIRECTION('ref_axis',(1.,0.,0.));
#21356=DIRECTION('center_axis',(0.,0.,1.));
#21357=DIRECTION('ref_axis',(1.,0.,0.));
#21358=DIRECTION('center_axis',(0.,0.,-1.));
#21359=DIRECTION('ref_axis',(-1.,0.,0.));
#21360=DIRECTION('center_axis',(0.,0.,1.));
#21361=DIRECTION('ref_axis',(1.,0.,0.));
#21362=DIRECTION('center_axis',(0.,0.,1.));
#21363=DIRECTION('ref_axis',(1.,0.,0.));
#21364=DIRECTION('',(0.707106781186547,8.65956056235493E-17,-0.707106781186548));
#21365=DIRECTION('center_axis',(0.,0.,-1.));
#21366=DIRECTION('ref_axis',(1.,0.,0.));
#21367=DIRECTION('center_axis',(0.,0.,1.));
#21368=DIRECTION('ref_axis',(1.,0.,0.));
#21369=DIRECTION('',(-0.707106781186547,-8.65956056235493E-17,-0.707106781186548));
#21370=DIRECTION('center_axis',(0.,0.,1.));
#21371=DIRECTION('ref_axis',(1.,0.,0.));
#21372=DIRECTION('axis',(0.,0.,1.));
#21373=DIRECTION('refdir',(1.,0.,0.));
#21374=DIRECTION('center_axis',(0.,0.,1.));
#21375=DIRECTION('ref_axis',(1.,0.,0.));
#21376=DIRECTION('',(0.,0.,-1.));
#21377=DIRECTION('center_axis',(0.,0.,1.));
#21378=DIRECTION('ref_axis',(1.,0.,0.));
#21379=DIRECTION('center_axis',(0.,0.,1.));
#21380=DIRECTION('ref_axis',(1.,0.,0.));
#21381=DIRECTION('',(0.,0.,-1.));
#21382=DIRECTION('center_axis',(0.,0.,1.));
#21383=DIRECTION('ref_axis',(1.,0.,0.));
#21384=DIRECTION('',(0.,0.,-1.));
#21385=DIRECTION('center_axis',(0.,0.,1.));
#21386=DIRECTION('ref_axis',(1.,0.,0.));
#21387=DIRECTION('',(0.,0.,-1.));
#21388=DIRECTION('center_axis',(0.,0.,1.));
#21389=DIRECTION('ref_axis',(1.,0.,0.));
#21390=DIRECTION('',(0.,0.,-1.));
#21391=DIRECTION('center_axis',(0.,0.,1.));
#21392=DIRECTION('ref_axis',(1.,0.,0.));
#21393=DIRECTION('',(0.,0.,-1.));
#21394=DIRECTION('center_axis',(0.,0.,1.));
#21395=DIRECTION('ref_axis',(1.,0.,0.));
#21396=DIRECTION('',(0.,0.,-1.));
#21397=DIRECTION('center_axis',(0.,0.,1.));
#21398=DIRECTION('ref_axis',(1.,0.,0.));
#21399=DIRECTION('',(0.,0.,-1.));
#21400=DIRECTION('center_axis',(0.,0.,1.));
#21401=DIRECTION('ref_axis',(1.,0.,0.));
#21402=DIRECTION('',(0.,0.,-1.));
#21403=DIRECTION('center_axis',(0.,0.,1.));
#21404=DIRECTION('ref_axis',(1.,0.,0.));
#21405=DIRECTION('',(0.,0.,-1.));
#21406=DIRECTION('center_axis',(0.,0.,1.));
#21407=DIRECTION('ref_axis',(1.,0.,0.));
#21408=DIRECTION('',(0.,0.,-1.));
#21409=DIRECTION('center_axis',(0.,0.,1.));
#21410=DIRECTION('ref_axis',(-0.266007747734115,-0.963970890714768,0.));
#21411=DIRECTION('',(0.,0.,1.));
#21412=DIRECTION('center_axis',(0.,0.,1.));
#21413=DIRECTION('ref_axis',(1.,5.3862180848358E-14,0.));
#21414=DIRECTION('center_axis',(0.,0.,1.));
#21415=DIRECTION('ref_axis',(1.,5.3862180848358E-14,0.));
#21416=DIRECTION('',(0.,0.,1.));
#21417=DIRECTION('center_axis',(0.,0.,1.));
#21418=DIRECTION('ref_axis',(1.,5.3862180848358E-14,0.));
#21419=DIRECTION('',(0.,0.,1.));
#21420=DIRECTION('center_axis',(0.,0.,1.));
#21421=DIRECTION('ref_axis',(1.,5.3862180848358E-14,0.));
#21422=DIRECTION('',(0.,0.,1.));
#21423=DIRECTION('center_axis',(0.,0.,1.));
#21424=DIRECTION('ref_axis',(1.,5.3862180848358E-14,0.));
#21425=DIRECTION('',(0.,0.,1.));
#21426=DIRECTION('center_axis',(0.,0.,1.));
#21427=DIRECTION('ref_axis',(1.,5.3862180848358E-14,0.));
#21428=DIRECTION('',(0.,0.,1.));
#21429=DIRECTION('center_axis',(0.,0.,1.));
#21430=DIRECTION('ref_axis',(1.,5.3862180848358E-14,0.));
#21431=DIRECTION('',(0.,0.,1.));
#21432=DIRECTION('center_axis',(0.,0.,1.));
#21433=DIRECTION('ref_axis',(1.,5.3862180848358E-14,0.));
#21434=DIRECTION('',(0.,0.,1.));
#21435=DIRECTION('center_axis',(0.,0.,1.));
#21436=DIRECTION('ref_axis',(1.,5.3862180848358E-14,0.));
#21437=DIRECTION('',(0.,0.,1.));
#21438=DIRECTION('center_axis',(0.,0.,1.));
#21439=DIRECTION('ref_axis',(1.,5.3862180848358E-14,0.));
#21440=DIRECTION('',(0.,0.,1.));
#21441=DIRECTION('center_axis',(0.,0.,1.));
#21442=DIRECTION('ref_axis',(1.,5.3862180848358E-14,0.));
#21443=DIRECTION('',(0.,0.,1.));
#21444=DIRECTION('center_axis',(0.,0.,1.));
#21445=DIRECTION('ref_axis',(1.,0.,0.));
#21446=DIRECTION('center_axis',(0.,0.,1.));
#21447=DIRECTION('ref_axis',(1.,0.,0.));
#21448=DIRECTION('center_axis',(0.,0.,1.));
#21449=DIRECTION('ref_axis',(1.,0.,0.));
#21450=DIRECTION('center_axis',(0.,0.,-1.));
#21451=DIRECTION('ref_axis',(1.,5.3862180848358E-14,0.));
#21452=DIRECTION('center_axis',(0.,0.,1.));
#21453=DIRECTION('ref_axis',(1.,5.3862180848358E-14,0.));
#21454=DIRECTION('center_axis',(0.0265854578674083,0.999646544249506,0.));
#21455=DIRECTION('ref_axis',(0.999646544249506,-0.0265854578674083,0.));
#21456=DIRECTION('',(0.,0.,-1.));
#21457=DIRECTION('',(0.,0.,-1.));
#21458=DIRECTION('center_axis',(-0.852426573191691,-0.522846954009173,0.));
#21459=DIRECTION('ref_axis',(-0.522846954009173,0.852426573191691,0.));
#21460=DIRECTION('',(0.,0.,1.));
#21461=DIRECTION('center_axis',(0.522846954009174,0.852426573191691,0.));
#21462=DIRECTION('ref_axis',(0.852426573191691,-0.522846954009174,0.));
#21463=DIRECTION('',(0.,0.,-1.));
#21464=DIRECTION('',(0.,0.,-1.));
#21465=DIRECTION('center_axis',(-0.999646544249506,-0.0265854578674079,
0.));
#21466=DIRECTION('ref_axis',(-0.0265854578674079,0.999646544249506,0.));
#21467=DIRECTION('',(0.,0.,1.));
#21468=DIRECTION('center_axis',(0.879012031059102,0.476799590240337,0.));
#21469=DIRECTION('ref_axis',(0.476799590240337,-0.879012031059102,0.));
#21470=DIRECTION('',(0.,0.,-1.));
#21471=DIRECTION('',(0.,0.,-1.));
#21472=DIRECTION('center_axis',(-0.879012031059104,0.476799590240333,0.));
#21473=DIRECTION('ref_axis',(0.476799590240333,0.879012031059104,0.));
#21474=DIRECTION('',(0.,0.,1.));
#21475=DIRECTION('center_axis',(0.999646544249506,-0.0265854578674083,0.));
#21476=DIRECTION('ref_axis',(-0.0265854578674083,-0.999646544249506,0.));
#21477=DIRECTION('',(0.,0.,-1.));
#21478=DIRECTION('',(0.,0.,-1.));
#21479=DIRECTION('center_axis',(-0.522846954009174,0.852426573191691,0.));
#21480=DIRECTION('ref_axis',(0.852426573191691,0.522846954009174,0.));
#21481=DIRECTION('',(0.,0.,1.));
#21482=DIRECTION('center_axis',(0.852426573191692,-0.522846954009172,0.));
#21483=DIRECTION('ref_axis',(-0.522846954009172,-0.852426573191692,0.));
#21484=DIRECTION('',(0.,0.,-1.));
#21485=DIRECTION('',(0.,0.,-1.));
#21486=DIRECTION('center_axis',(-0.026585457867411,0.999646544249506,0.));
#21487=DIRECTION('ref_axis',(0.999646544249506,0.026585457867411,0.));
#21488=DIRECTION('',(0.,0.,1.));
#21489=DIRECTION('center_axis',(0.476799590240335,-0.879012031059103,0.));
#21490=DIRECTION('ref_axis',(-0.879012031059103,-0.476799590240335,0.));
#21491=DIRECTION('',(0.,0.,-1.));
#21492=DIRECTION('',(0.,0.,-1.));
#21493=DIRECTION('center_axis',(0.476799590240335,0.879012031059103,0.));
#21494=DIRECTION('ref_axis',(0.879012031059103,-0.476799590240335,0.));
#21495=DIRECTION('',(0.,0.,1.));
#21496=DIRECTION('center_axis',(0.23304798366484,-0.972465237070073,0.));
#21497=DIRECTION('ref_axis',(-0.972465237070073,-0.23304798366484,0.));
#21498=DIRECTION('',(0.,0.,-1.));
#21499=DIRECTION('',(0.,0.,-1.));
#21500=DIRECTION('center_axis',(0.688058092689529,0.725655607767519,0.));
#21501=DIRECTION('ref_axis',(0.725655607767519,-0.688058092689529,0.));
#21502=DIRECTION('',(0.,0.,1.));
#21503=DIRECTION('center_axis',(-0.284407144380544,-0.958703591432359,0.));
#21504=DIRECTION('ref_axis',(-0.958703591432359,0.284407144380544,0.));
#21505=DIRECTION('',(0.,0.,-1.));
#21506=DIRECTION('',(0.,0.,-1.));
#21507=DIRECTION('center_axis',(0.95870359143236,0.284407144380544,0.));
#21508=DIRECTION('ref_axis',(0.284407144380544,-0.95870359143236,0.));
#21509=DIRECTION('',(0.,0.,1.));
#21510=DIRECTION('center_axis',(-0.725655607767519,-0.688058092689529,0.));
#21511=DIRECTION('ref_axis',(-0.688058092689529,0.725655607767519,0.));
#21512=DIRECTION('',(0.,0.,-1.));
#21513=DIRECTION('',(0.,0.,-1.));
#21514=DIRECTION('center_axis',(0.972465237070073,-0.23304798366484,0.));
#21515=DIRECTION('ref_axis',(-0.23304798366484,-0.972465237070073,0.));
#21516=DIRECTION('',(0.,0.,1.));
#21517=DIRECTION('center_axis',(-0.972465237070073,-0.23304798366484,0.));
#21518=DIRECTION('ref_axis',(-0.23304798366484,0.972465237070073,0.));
#21519=DIRECTION('',(0.,0.,-1.));
#21520=DIRECTION('',(0.,0.,-1.));
#21521=DIRECTION('center_axis',(0.725655607767519,-0.688058092689529,0.));
#21522=DIRECTION('ref_axis',(-0.688058092689529,-0.725655607767519,0.));
#21523=DIRECTION('',(0.,0.,1.));
#21524=DIRECTION('center_axis',(-0.95870359143236,0.284407144380544,0.));
#21525=DIRECTION('ref_axis',(0.284407144380544,0.95870359143236,0.));
#21526=DIRECTION('',(0.,0.,-1.));
#21527=DIRECTION('',(0.,0.,-1.));
#21528=DIRECTION('center_axis',(0.284407144380544,-0.95870359143236,0.));
#21529=DIRECTION('ref_axis',(-0.95870359143236,-0.284407144380544,0.));
#21530=DIRECTION('',(0.,0.,1.));
#21531=DIRECTION('center_axis',(-0.688058092689529,0.725655607767519,0.));
#21532=DIRECTION('ref_axis',(0.725655607767519,0.688058092689529,0.));
#21533=DIRECTION('',(0.,0.,-1.));
#21534=DIRECTION('',(0.,0.,-1.));
#21535=DIRECTION('center_axis',(-0.23304798366484,-0.972465237070073,0.));
#21536=DIRECTION('ref_axis',(-0.972465237070073,0.23304798366484,0.));
#21537=DIRECTION('',(0.,0.,1.));
#21538=DIRECTION('center_axis',(-0.852426573191692,0.522846954009171,0.));
#21539=DIRECTION('ref_axis',(0.522846954009171,0.852426573191692,0.));
#21540=DIRECTION('',(0.,0.,-1.));
#21541=DIRECTION('',(0.,0.,-1.));
#21542=DIRECTION('center_axis',(0.026585457867411,-0.999646544249506,0.));
#21543=DIRECTION('ref_axis',(-0.999646544249506,-0.026585457867411,0.));
#21544=DIRECTION('',(0.,0.,1.));
#21545=DIRECTION('center_axis',(-0.999646544249506,0.0265854578674102,0.));
#21546=DIRECTION('ref_axis',(0.0265854578674102,0.999646544249506,0.));
#21547=DIRECTION('',(0.,0.,-1.));
#21548=DIRECTION('',(0.,0.,-1.));
#21549=DIRECTION('center_axis',(0.522846954009173,-0.852426573191692,0.));
#21550=DIRECTION('ref_axis',(-0.852426573191692,-0.522846954009173,0.));
#21551=DIRECTION('',(0.,0.,1.));
#21552=DIRECTION('center_axis',(-0.879012031059103,-0.476799590240335,0.));
#21553=DIRECTION('ref_axis',(-0.476799590240335,0.879012031059103,0.));
#21554=DIRECTION('',(0.,0.,-1.));
#21555=DIRECTION('',(0.,0.,-1.));
#21556=DIRECTION('center_axis',(0.879012031059103,-0.476799590240335,0.));
#21557=DIRECTION('ref_axis',(-0.476799590240335,-0.879012031059103,0.));
#21558=DIRECTION('',(0.,0.,1.));
#21559=DIRECTION('center_axis',(-0.522846954009172,-0.852426573191692,0.));
#21560=DIRECTION('ref_axis',(-0.852426573191692,0.522846954009172,0.));
#21561=DIRECTION('',(0.,0.,-1.));
#21562=DIRECTION('',(0.,0.,-1.));
#21563=DIRECTION('center_axis',(0.999646544249506,0.0265854578674102,0.));
#21564=DIRECTION('ref_axis',(0.0265854578674102,-0.999646544249506,0.));
#21565=DIRECTION('',(0.,0.,1.));
#21566=DIRECTION('center_axis',(-0.0265854578674106,-0.999646544249506,
0.));
#21567=DIRECTION('ref_axis',(-0.999646544249506,0.0265854578674106,0.));
#21568=DIRECTION('',(0.,0.,-1.));
#21569=DIRECTION('',(0.,0.,-1.));
#21570=DIRECTION('center_axis',(0.852426573191692,0.522846954009171,0.));
#21571=DIRECTION('ref_axis',(0.522846954009171,-0.852426573191692,0.));
#21572=DIRECTION('',(0.,0.,1.));
#21573=DIRECTION('center_axis',(-0.476799590240335,0.879012031059103,0.));
#21574=DIRECTION('ref_axis',(0.879012031059103,0.476799590240335,0.));
#21575=DIRECTION('',(0.,0.,-1.));
#21576=DIRECTION('',(0.,0.,-1.));
#21577=DIRECTION('center_axis',(-0.476799590240335,-0.879012031059103,0.));
#21578=DIRECTION('ref_axis',(-0.879012031059103,0.476799590240335,0.));
#21579=DIRECTION('',(0.,0.,1.));
#21580=DIRECTION('center_axis',(0.688058092689529,-0.725655607767519,0.));
#21581=DIRECTION('ref_axis',(-0.725655607767519,-0.688058092689529,0.));
#21582=DIRECTION('',(0.,0.,-1.));
#21583=DIRECTION('',(0.,0.,-1.));
#21584=DIRECTION('center_axis',(0.23304798366484,0.972465237070073,0.));
#21585=DIRECTION('ref_axis',(0.972465237070073,-0.23304798366484,0.));
#21586=DIRECTION('',(0.,0.,1.));
#21587=DIRECTION('center_axis',(0.95870359143236,-0.284407144380542,0.));
#21588=DIRECTION('ref_axis',(-0.284407144380542,-0.95870359143236,0.));
#21589=DIRECTION('',(0.,0.,-1.));
#21590=DIRECTION('',(0.,0.,-1.));
#21591=DIRECTION('center_axis',(-0.284407144380544,0.95870359143236,0.));
#21592=DIRECTION('ref_axis',(0.95870359143236,0.284407144380544,0.));
#21593=DIRECTION('',(0.,0.,1.));
#21594=DIRECTION('center_axis',(0.972465237070073,0.233047983664838,0.));
#21595=DIRECTION('ref_axis',(0.233047983664838,-0.972465237070073,0.));
#21596=DIRECTION('',(0.,0.,-1.));
#21597=DIRECTION('',(0.,0.,-1.));
#21598=DIRECTION('center_axis',(-0.725655607767518,0.688058092689531,0.));
#21599=DIRECTION('ref_axis',(0.688058092689531,0.725655607767518,0.));
#21600=DIRECTION('',(0.,0.,1.));
#21601=DIRECTION('center_axis',(0.725655607767518,0.688058092689531,0.));
#21602=DIRECTION('ref_axis',(0.688058092689531,-0.725655607767518,0.));
#21603=DIRECTION('',(0.,0.,-1.));
#21604=DIRECTION('',(0.,0.,-1.));
#21605=DIRECTION('center_axis',(-0.972465237070073,0.233047983664838,0.));
#21606=DIRECTION('ref_axis',(0.233047983664838,0.972465237070073,0.));
#21607=DIRECTION('',(0.,0.,1.));
#21608=DIRECTION('center_axis',(0.284407144380542,0.95870359143236,0.));
#21609=DIRECTION('ref_axis',(0.95870359143236,-0.284407144380542,0.));
#21610=DIRECTION('',(0.,0.,-1.));
#21611=DIRECTION('',(0.,0.,-1.));
#21612=DIRECTION('center_axis',(-0.958703591432359,-0.284407144380547,0.));
#21613=DIRECTION('ref_axis',(-0.284407144380547,0.958703591432359,0.));
#21614=DIRECTION('',(0.,0.,1.));
#21615=DIRECTION('center_axis',(-0.233047983664838,0.972465237070073,0.));
#21616=DIRECTION('ref_axis',(0.972465237070073,0.233047983664838,0.));
#21617=DIRECTION('',(0.,0.,-1.));
#21618=DIRECTION('',(0.,0.,-1.));
#21619=DIRECTION('center_axis',(-0.688058092689531,-0.725655607767518,0.));
#21620=DIRECTION('ref_axis',(-0.725655607767518,0.688058092689531,0.));
#21621=DIRECTION('',(0.,0.,1.));
#21622=DIRECTION('center_axis',(0.,0.,1.));
#21623=DIRECTION('ref_axis',(1.,0.,0.));
#21624=DIRECTION('center_axis',(0.,0.,1.));
#21625=DIRECTION('ref_axis',(1.,0.,0.));
#21626=DIRECTION('center_axis',(0.,0.,1.));
#21627=DIRECTION('ref_axis',(1.,0.,0.));
#21628=DIRECTION('center_axis',(0.,0.,1.));
#21629=DIRECTION('ref_axis',(1.,0.,0.));
#21630=DIRECTION('center_axis',(0.,0.,1.));
#21631=DIRECTION('ref_axis',(1.,0.,0.));
#21632=DIRECTION('center_axis',(0.,0.,1.));
#21633=DIRECTION('ref_axis',(1.,0.,0.));
#21634=DIRECTION('center_axis',(0.,0.,1.));
#21635=DIRECTION('ref_axis',(1.,0.,0.));
#21636=DIRECTION('center_axis',(0.,0.,1.));
#21637=DIRECTION('ref_axis',(1.,0.,0.));
#21638=DIRECTION('center_axis',(0.,0.,1.));
#21639=DIRECTION('ref_axis',(1.,0.,0.));
#21640=DIRECTION('center_axis',(0.,0.,1.));
#21641=DIRECTION('ref_axis',(1.,0.,0.));
#21642=DIRECTION('center_axis',(0.,0.,1.));
#21643=DIRECTION('ref_axis',(1.,0.,0.));
#21644=DIRECTION('center_axis',(0.,0.,1.));
#21645=DIRECTION('ref_axis',(1.,0.,0.));
#21646=DIRECTION('center_axis',(0.,0.,1.));
#21647=DIRECTION('ref_axis',(1.,0.,0.));
#21648=DIRECTION('center_axis',(0.,0.,1.));
#21649=DIRECTION('ref_axis',(1.,0.,0.));
#21650=DIRECTION('center_axis',(0.,0.,1.));
#21651=DIRECTION('ref_axis',(1.,0.,0.));
#21652=DIRECTION('center_axis',(0.,0.,1.));
#21653=DIRECTION('ref_axis',(1.,0.,0.));
#21654=DIRECTION('center_axis',(0.,0.,1.));
#21655=DIRECTION('ref_axis',(1.,0.,0.));
#21656=DIRECTION('center_axis',(0.,0.,1.));
#21657=DIRECTION('ref_axis',(1.,0.,0.));
#21658=DIRECTION('center_axis',(0.,0.,1.));
#21659=DIRECTION('ref_axis',(1.,0.,0.));
#21660=DIRECTION('center_axis',(0.,0.,1.));
#21661=DIRECTION('ref_axis',(1.,0.,0.));
#21662=DIRECTION('center_axis',(0.,0.,1.));
#21663=DIRECTION('ref_axis',(1.,0.,0.));
#21664=DIRECTION('center_axis',(0.,0.,1.));
#21665=DIRECTION('ref_axis',(1.,0.,0.));
#21666=DIRECTION('center_axis',(0.,0.,1.));
#21667=DIRECTION('ref_axis',(1.,0.,0.));
#21668=DIRECTION('center_axis',(0.,0.,1.));
#21669=DIRECTION('ref_axis',(1.,0.,0.));
#21670=DIRECTION('center_axis',(0.,0.,1.));
#21671=DIRECTION('ref_axis',(1.,0.,0.));
#21672=DIRECTION('center_axis',(0.,0.,1.));
#21673=DIRECTION('ref_axis',(1.,0.,0.));
#21674=DIRECTION('center_axis',(0.,0.,1.));
#21675=DIRECTION('ref_axis',(1.,0.,0.));
#21676=DIRECTION('center_axis',(0.,0.,1.));
#21677=DIRECTION('ref_axis',(1.,0.,0.));
#21678=DIRECTION('center_axis',(0.,0.,1.));
#21679=DIRECTION('ref_axis',(1.,0.,0.));
#21680=DIRECTION('center_axis',(0.,0.,1.));
#21681=DIRECTION('ref_axis',(1.,0.,0.));
#21682=DIRECTION('center_axis',(0.,0.,1.));
#21683=DIRECTION('ref_axis',(1.,0.,0.));
#21684=DIRECTION('center_axis',(0.,0.,1.));
#21685=DIRECTION('ref_axis',(1.,0.,0.));
#21686=DIRECTION('center_axis',(0.,0.,1.));
#21687=DIRECTION('ref_axis',(1.,0.,0.));
#21688=DIRECTION('center_axis',(0.,0.,1.));
#21689=DIRECTION('ref_axis',(1.,0.,0.));
#21690=DIRECTION('center_axis',(0.,0.,1.));
#21691=DIRECTION('ref_axis',(1.,0.,0.));
#21692=DIRECTION('center_axis',(0.,0.,1.));
#21693=DIRECTION('ref_axis',(1.,0.,0.));
#21694=DIRECTION('center_axis',(0.,0.,1.));
#21695=DIRECTION('ref_axis',(1.,0.,0.));
#21696=DIRECTION('center_axis',(0.,0.,1.));
#21697=DIRECTION('ref_axis',(1.,0.,0.));
#21698=DIRECTION('center_axis',(0.,0.,1.));
#21699=DIRECTION('ref_axis',(1.,0.,0.));
#21700=DIRECTION('center_axis',(0.,0.,1.));
#21701=DIRECTION('ref_axis',(1.,0.,0.));
#21702=DIRECTION('center_axis',(0.,0.,1.));
#21703=DIRECTION('ref_axis',(1.,0.,0.));
#21704=DIRECTION('center_axis',(0.,0.,1.));
#21705=DIRECTION('ref_axis',(1.,0.,0.));
#21706=DIRECTION('center_axis',(0.,0.,1.));
#21707=DIRECTION('ref_axis',(1.,0.,0.));
#21708=DIRECTION('center_axis',(0.,0.,1.));
#21709=DIRECTION('ref_axis',(1.,0.,0.));
#21710=DIRECTION('center_axis',(0.,0.,1.));
#21711=DIRECTION('ref_axis',(1.,0.,0.));
#21712=DIRECTION('center_axis',(0.,0.,1.));
#21713=DIRECTION('ref_axis',(1.,0.,0.));
#21714=DIRECTION('center_axis',(0.,0.,1.));
#21715=DIRECTION('ref_axis',(1.,0.,0.));
#21716=DIRECTION('center_axis',(0.,0.,1.));
#21717=DIRECTION('ref_axis',(1.,0.,0.));
#21718=DIRECTION('center_axis',(0.,0.,1.));
#21719=DIRECTION('ref_axis',(1.,0.,0.));
#21720=DIRECTION('center_axis',(0.,0.,1.));
#21721=DIRECTION('ref_axis',(1.,0.,0.));
#21722=DIRECTION('center_axis',(0.,0.,1.));
#21723=DIRECTION('ref_axis',(1.,0.,0.));
#21724=DIRECTION('center_axis',(0.,0.,1.));
#21725=DIRECTION('ref_axis',(1.,0.,0.));
#21726=DIRECTION('center_axis',(0.,0.,1.));
#21727=DIRECTION('ref_axis',(1.,0.,0.));
#21728=DIRECTION('center_axis',(0.,0.,1.));
#21729=DIRECTION('ref_axis',(1.,0.,0.));
#21730=DIRECTION('center_axis',(0.,0.,1.));
#21731=DIRECTION('ref_axis',(1.,0.,0.));
#21732=DIRECTION('center_axis',(0.,0.,1.));
#21733=DIRECTION('ref_axis',(1.,0.,0.));
#21734=DIRECTION('center_axis',(0.,0.,1.));
#21735=DIRECTION('ref_axis',(1.,0.,0.));
#21736=DIRECTION('center_axis',(0.,0.,1.));
#21737=DIRECTION('ref_axis',(1.,0.,0.));
#21738=DIRECTION('center_axis',(0.,0.,1.));
#21739=DIRECTION('ref_axis',(1.,0.,0.));
#21740=DIRECTION('center_axis',(0.,0.,1.));
#21741=DIRECTION('ref_axis',(1.,0.,0.));
#21742=DIRECTION('center_axis',(0.,0.,1.));
#21743=DIRECTION('ref_axis',(1.,0.,0.));
#21744=DIRECTION('center_axis',(0.,0.,1.));
#21745=DIRECTION('ref_axis',(1.,0.,0.));
#21746=DIRECTION('center_axis',(0.,0.,1.));
#21747=DIRECTION('ref_axis',(1.,0.,0.));
#21748=DIRECTION('center_axis',(0.,0.,1.));
#21749=DIRECTION('ref_axis',(1.,0.,0.));
#21750=DIRECTION('center_axis',(0.,0.,1.));
#21751=DIRECTION('ref_axis',(1.,0.,0.));
#21752=DIRECTION('center_axis',(0.,0.,1.));
#21753=DIRECTION('ref_axis',(1.,0.,0.));
#21754=DIRECTION('center_axis',(0.,0.,1.));
#21755=DIRECTION('ref_axis',(1.,0.,0.));
#21756=DIRECTION('center_axis',(0.,0.,1.));
#21757=DIRECTION('ref_axis',(1.,0.,0.));
#21758=DIRECTION('center_axis',(0.,0.,1.));
#21759=DIRECTION('ref_axis',(1.,0.,0.));
#21760=DIRECTION('center_axis',(0.,0.,1.));
#21761=DIRECTION('ref_axis',(1.,0.,0.));
#21762=DIRECTION('center_axis',(0.,0.,1.));
#21763=DIRECTION('ref_axis',(1.,0.,0.));
#21764=DIRECTION('center_axis',(0.,0.,1.));
#21765=DIRECTION('ref_axis',(1.,0.,0.));
#21766=DIRECTION('center_axis',(0.,0.,1.));
#21767=DIRECTION('ref_axis',(1.,0.,0.));
#21768=DIRECTION('',(0.707106781186548,8.65956056235494E-17,-0.707106781186547));
#21769=DIRECTION('center_axis',(0.,0.,1.));
#21770=DIRECTION('ref_axis',(1.,0.,0.));
#21771=DIRECTION('center_axis',(0.,0.,-1.));
#21772=DIRECTION('ref_axis',(-1.,0.,0.));
#21773=DIRECTION('center_axis',(0.,0.,1.));
#21774=DIRECTION('ref_axis',(1.,0.,0.));
#21775=DIRECTION('center_axis',(0.,0.,1.));
#21776=DIRECTION('ref_axis',(1.,0.,0.));
#21777=DIRECTION('',(0.707106781186547,8.65956056235493E-17,-0.707106781186547));
#21778=DIRECTION('center_axis',(0.,0.,1.));
#21779=DIRECTION('ref_axis',(0.939073945770631,-0.343715179145143,0.));
#21780=DIRECTION('center_axis',(0.,0.,1.));
#21781=DIRECTION('ref_axis',(1.,0.,0.));
#21782=DIRECTION('center_axis',(0.,0.,-1.));
#21783=DIRECTION('ref_axis',(-1.,0.,0.));
#21784=DIRECTION('center_axis',(0.,0.,-1.));
#21785=DIRECTION('ref_axis',(1.,0.,0.));
#21786=DIRECTION('center_axis',(0.,0.,1.));
#21787=DIRECTION('ref_axis',(1.,0.,0.));
#21788=DIRECTION('',(-0.707106781186548,-8.65956056235494E-17,-0.707106781186547));
#21789=DIRECTION('center_axis',(0.,0.,1.));
#21790=DIRECTION('ref_axis',(1.,0.,0.));
#21791=DIRECTION('',(0.,0.,1.));
#21792=DIRECTION('',(1.,0.,0.));
#21793=DIRECTION('',(0.,0.,1.));
#21794=DIRECTION('',(1.,0.,0.));
#21795=DIRECTION('',(0.,0.,1.));
#21796=DIRECTION('',(1.,0.,0.));
#21797=DIRECTION('',(0.,0.,1.));
#21798=DIRECTION('',(1.,0.,0.));
#21799=DIRECTION('',(0.,0.,1.));
#21800=DIRECTION('',(1.,0.,0.));
#21801=DIRECTION('',(0.,0.,1.));
#21802=DIRECTION('',(1.,0.,0.));
#21803=DIRECTION('',(6.29018434530969E-235,-1.,-2.22044604925031E-16));
#21804=DIRECTION('',(1.,0.,0.));
#21805=DIRECTION('',(0.,0.,1.));
#21806=DIRECTION('',(1.,0.,0.));
#21807=DIRECTION('',(0.,-1.,-2.22044604925031E-16));
#21808=DIRECTION('',(1.,0.,0.));
#21809=DIRECTION('',(0.,-1.,-2.22044604925031E-16));
#21810=DIRECTION('',(1.,0.,0.));
#21811=DIRECTION('',(0.,-1.,-2.22044604925031E-16));
#21812=DIRECTION('',(1.,0.,0.));
#21813=DIRECTION('',(0.,1.,-2.22044604925031E-16));
#21814=DIRECTION('',(1.,0.,0.));
#21815=DIRECTION('',(0.,1.,-2.22044604925031E-16));
#21816=DIRECTION('',(1.,0.,0.));
#21817=DIRECTION('',(0.,0.,1.));
#21818=DIRECTION('',(1.,0.,0.));
#21819=DIRECTION('',(6.29018434530969E-235,-1.,-2.22044604925031E-16));
#21820=DIRECTION('',(1.,0.,0.));
#21821=DIRECTION('',(6.29018434530969E-235,-1.,-2.22044604925031E-16));
#21822=DIRECTION('',(1.,0.,0.));
#21823=DIRECTION('',(0.,0.,1.));
#21824=DIRECTION('',(1.,0.,0.));
#21825=DIRECTION('',(0.,0.,1.));
#21826=DIRECTION('',(1.,0.,0.));
#21827=DIRECTION('',(0.,-1.,-2.22044604925031E-16));
#21828=DIRECTION('',(1.,0.,0.));
#21829=DIRECTION('',(0.,-1.,-2.22044604925031E-16));
#21830=DIRECTION('',(1.,0.,0.));
#21831=DIRECTION('',(-1.,2.22044604925031E-16,-2.22044604925031E-16));
#21832=DIRECTION('',(-2.22044604925031E-16,-1.,0.));
#21833=CARTESIAN_POINT('',(0.,0.,0.));
#21834=CARTESIAN_POINT('',(0.,0.,0.));
#21835=CARTESIAN_POINT('Origin',(3.985,-1.16,0.4));
#21836=CARTESIAN_POINT('',(3.985,-1.16,0.0250000000000002));
#21837=CARTESIAN_POINT('',(4.,-1.145,0.04));
#21838=CARTESIAN_POINT('',(3.98916666666667,-1.15583333333333,0.0291666666666659));
#21839=CARTESIAN_POINT('',(4.,-1.145,0.74));
#21840=CARTESIAN_POINT('',(4.,-1.145,0.4));
#21841=CARTESIAN_POINT('',(3.985,-1.16,0.755));
#21842=CARTESIAN_POINT('',(3.9825,-1.1625,0.757500000000001));
#21843=CARTESIAN_POINT('',(3.97,-1.175,0.74));
#21844=CARTESIAN_POINT('',(3.44166666666668,-1.70333333333333,0.211666666666669));
#21845=CARTESIAN_POINT('',(3.97,-1.175,0.04));
#21846=CARTESIAN_POINT('',(3.97,-1.175,0.4));
#21847=CARTESIAN_POINT('',(3.43500000000001,-1.71,0.574999999999998));
#21848=CARTESIAN_POINT('Origin',(1.05,-1.145,0.77));
#21849=CARTESIAN_POINT('',(3.9612132034356,-1.1362132034356,0.778786796564403));
#21850=CARTESIAN_POINT('',(3.94,-1.115,0.8));
#21851=CARTESIAN_POINT('',(2.1,-1.1362132034356,0.778786796564404));
#21852=CARTESIAN_POINT('',(0.525,-1.1362132034356,0.778786796564404));
#21853=CARTESIAN_POINT('',(2.1,-1.175,0.74));
#21854=CARTESIAN_POINT('',(2.1,-1.175,0.74));
#21855=CARTESIAN_POINT('',(1.05,-1.175,0.74));
#21856=CARTESIAN_POINT('Origin',(3.97,-1.5,0.77));
#21857=CARTESIAN_POINT('',(4.,1.145,0.74));
#21858=CARTESIAN_POINT('',(4.,-1.5,0.74));
#21859=CARTESIAN_POINT('',(3.985,1.16,0.755));
#21860=CARTESIAN_POINT('',(4.4825,0.662499999999977,0.257499999999996));
#21861=CARTESIAN_POINT('',(3.9612132034356,1.1362132034356,0.778786796564404));
#21862=CARTESIAN_POINT('',(3.94,1.115,0.8));
#21863=CARTESIAN_POINT('',(3.9612132034356,-0.75,0.778786796564403));
#21864=CARTESIAN_POINT('Origin',(4.,-3.,0.));
#21865=CARTESIAN_POINT('',(4.,1.145,0.04));
#21866=CARTESIAN_POINT('',(4.,-1.5,0.04));
#21867=CARTESIAN_POINT('',(4.,1.145,0.4));
#21868=CARTESIAN_POINT('Origin',(3.985,1.16,0.4));
#21869=CARTESIAN_POINT('',(3.985,1.16,0.0250000000000001));
#21870=CARTESIAN_POINT('',(4.48916666666667,0.65583333333331,0.52916666666667));
#21871=CARTESIAN_POINT('',(3.97,1.175,0.04));
#21872=CARTESIAN_POINT('',(3.60166666666668,1.54333333333333,0.408333333333331));
#21873=CARTESIAN_POINT('',(3.97,1.175,0.74));
#21874=CARTESIAN_POINT('',(3.97,1.175,0.4));
#21875=CARTESIAN_POINT('',(3.60833333333335,1.53666666666666,0.378333333333336));
#21876=CARTESIAN_POINT('Origin',(2.05,1.145,0.77));
#21877=CARTESIAN_POINT('',(2.1,1.175,0.74));
#21878=CARTESIAN_POINT('',(2.05,1.175,0.74));
#21879=CARTESIAN_POINT('',(2.1,1.1362132034356,0.778786796564404));
#21880=CARTESIAN_POINT('',(2.1,1.175,0.74));
#21881=CARTESIAN_POINT('',(1.025,1.1362132034356,0.778786796564404));
#21882=CARTESIAN_POINT('Origin',(3.985,-1.84,0.4));
#21883=CARTESIAN_POINT('',(3.985,-1.84,0.755));
#21884=CARTESIAN_POINT('',(4.,-1.855,0.74));
#21885=CARTESIAN_POINT('',(3.9825,-1.8375,0.757500000000001));
#21886=CARTESIAN_POINT('',(4.,-1.855,0.04));
#21887=CARTESIAN_POINT('',(4.,-1.855,0.4));
#21888=CARTESIAN_POINT('',(3.985,-1.84,0.0250000000000002));
#21889=CARTESIAN_POINT('',(3.98916666666666,-1.84416666666666,0.029166666666665));
#21890=CARTESIAN_POINT('',(3.97,-1.825,0.04));
#21891=CARTESIAN_POINT('',(3.60166666666668,-1.45666666666667,0.408333333333331));
#21892=CARTESIAN_POINT('',(3.97,-1.825,0.74));
#21893=CARTESIAN_POINT('',(3.97,-1.825,0.4));
#21894=CARTESIAN_POINT('',(3.60833333333335,-1.46333333333334,0.378333333333335));
#21895=CARTESIAN_POINT('Origin',(4.,-3.,0.));
#21896=CARTESIAN_POINT('',(4.,-2.6,0.74));
#21897=CARTESIAN_POINT('',(4.,-1.5,0.74));
#21898=CARTESIAN_POINT('',(4.,-2.6,0.04));
#21899=CARTESIAN_POINT('',(4.,-2.6,0.));
#21900=CARTESIAN_POINT('',(4.,-1.5,0.04));
#21901=CARTESIAN_POINT('Origin',(3.97,-1.5,0.77));
#21902=CARTESIAN_POINT('',(3.9612132034356,-1.8637867965644,0.778786796564404));
#21903=CARTESIAN_POINT('',(3.94,-1.885,0.8));
#21904=CARTESIAN_POINT('',(3.9612132034356,-2.6,0.778786796564403));
#21905=CARTESIAN_POINT('',(3.9612132034356,-0.75,0.778786796564403));
#21906=CARTESIAN_POINT('',(4.,-2.6,0.74));
#21907=CARTESIAN_POINT('Origin',(2.05,-1.855,0.77));
#21908=CARTESIAN_POINT('',(2.1,-1.825,0.74));
#21909=CARTESIAN_POINT('',(2.05,-1.825,0.74));
#21910=CARTESIAN_POINT('',(2.1,-1.8637867965644,0.778786796564404));
#21911=CARTESIAN_POINT('',(2.1,-1.825,0.74));
#21912=CARTESIAN_POINT('',(1.025,-1.8637867965644,0.778786796564404));
#21913=CARTESIAN_POINT('Origin',(-3.985,-1.84,0.4));
#21914=CARTESIAN_POINT('',(-3.985,-1.84,0.0250000000000001));
#21915=CARTESIAN_POINT('',(-4.,-1.855,0.04));
#21916=CARTESIAN_POINT('',(-3.48916666666666,-1.34416666666665,-0.470833333333338));
#21917=CARTESIAN_POINT('',(-4.,-1.855,0.74));
#21918=CARTESIAN_POINT('',(-4.,-1.855,0.4));
#21919=CARTESIAN_POINT('',(-3.985,-1.84,0.755));
#21920=CARTESIAN_POINT('',(-3.4825,-1.33749999999998,1.2575));
#21921=CARTESIAN_POINT('',(-3.97,-1.825,0.74));
#21922=CARTESIAN_POINT('',(-3.44166666666668,-1.29666666666667,0.21166666666667));
#21923=CARTESIAN_POINT('',(-3.97,-1.825,0.04));
#21924=CARTESIAN_POINT('',(-3.97,-1.825,0.4));
#21925=CARTESIAN_POINT('',(-3.43500000000002,-1.29,0.574999999999997));
#21926=CARTESIAN_POINT('Origin',(-3.97,1.5,0.77));
#21927=CARTESIAN_POINT('',(-4.,-2.6,0.74));
#21928=CARTESIAN_POINT('',(-4.,1.5,0.74));
#21929=CARTESIAN_POINT('',(-3.9612132034356,-2.6,0.778786796564404));
#21930=CARTESIAN_POINT('',(-4.,-2.6,0.74));
#21931=CARTESIAN_POINT('',(-3.9612132034356,-1.8637867965644,0.778786796564403));
#21932=CARTESIAN_POINT('',(-3.9612132034356,0.75,0.778786796564403));
#21933=CARTESIAN_POINT('',(-3.94,-1.885,0.8));
#21934=CARTESIAN_POINT('Origin',(-4.,3.,0.));
#21935=CARTESIAN_POINT('',(-4.,-2.6,0.04));
#21936=CARTESIAN_POINT('',(-4.,1.5,0.04));
#21937=CARTESIAN_POINT('',(-4.,-2.6,0.));
#21938=CARTESIAN_POINT('Origin',(-3.98,1.5,0.02));
#21939=CARTESIAN_POINT('',(-3.96,-1.865,0.));
#21940=CARTESIAN_POINT('',(-4.,-1.825,0.04));
#21941=CARTESIAN_POINT('',(-3.96,-2.6,0.));
#21942=CARTESIAN_POINT('',(-3.96,1.5,0.));
#21943=CARTESIAN_POINT('',(-3.96,-2.6,0.));
#21944=CARTESIAN_POINT('Origin',(-3.985,-1.16,0.4));
#21945=CARTESIAN_POINT('',(-3.985,-1.16,0.755));
#21946=CARTESIAN_POINT('',(-4.,-1.145,0.74));
#21947=CARTESIAN_POINT('',(-4.4825,-0.662499999999977,0.257499999999996));
#21948=CARTESIAN_POINT('',(-4.,-1.145,0.04));
#21949=CARTESIAN_POINT('',(-4.,-1.145,0.4));
#21950=CARTESIAN_POINT('',(-3.985,-1.16,0.0250000000000001));
#21951=CARTESIAN_POINT('',(-4.48916666666667,-0.65583333333331,0.52916666666667));
#21952=CARTESIAN_POINT('',(-3.97,-1.175,0.04));
#21953=CARTESIAN_POINT('',(-3.60166666666668,-1.54333333333333,0.408333333333331));
#21954=CARTESIAN_POINT('',(-3.97,-1.175,0.74));
#21955=CARTESIAN_POINT('',(-3.97,-1.175,0.4));
#21956=CARTESIAN_POINT('',(-3.60833333333335,-1.53666666666666,0.378333333333336));
#21957=CARTESIAN_POINT('Origin',(-3.98,1.5,0.02));
#21958=CARTESIAN_POINT('',(-4.,1.145,0.04));
#21959=CARTESIAN_POINT('',(-4.,1.5,0.04));
#21960=CARTESIAN_POINT('',(-3.985,1.16,0.0250000000000002));
#21961=CARTESIAN_POINT('',(-3.98916666666667,1.15583333333333,0.0291666666666659));
#21962=CARTESIAN_POINT('',(-3.96,1.135,0.));
#21963=CARTESIAN_POINT('',(-4.,1.175,0.04));
#21964=CARTESIAN_POINT('',(-3.96,-1.135,0.));
#21965=CARTESIAN_POINT('',(-3.96,1.5,0.));
#21966=CARTESIAN_POINT('',(-3.96,-1.135,0.));
#21967=CARTESIAN_POINT('Origin',(-4.,3.,0.));
#21968=CARTESIAN_POINT('',(-4.,1.145,0.74));
#21969=CARTESIAN_POINT('',(-4.,1.5,0.74));
#21970=CARTESIAN_POINT('',(-4.,1.145,0.4));
#21971=CARTESIAN_POINT('Origin',(-3.97,1.5,0.77));
#21972=CARTESIAN_POINT('',(-3.9612132034356,-1.1362132034356,0.778786796564404));
#21973=CARTESIAN_POINT('',(-3.94,-1.115,0.8));
#21974=CARTESIAN_POINT('',(-3.9612132034356,1.1362132034356,0.778786796564403));
#21975=CARTESIAN_POINT('',(-3.9612132034356,0.75,0.778786796564403));
#21976=CARTESIAN_POINT('',(-3.985,1.16,0.755));
#21977=CARTESIAN_POINT('',(-3.94,1.115,0.8));
#21978=CARTESIAN_POINT('',(-3.9825,1.1625,0.757500000000001));
#21979=CARTESIAN_POINT('Origin',(-3.985,1.16,0.4));
#21980=CARTESIAN_POINT('',(-3.97,1.175,0.74));
#21981=CARTESIAN_POINT('',(-3.44166666666668,1.70333333333333,0.211666666666669));
#21982=CARTESIAN_POINT('',(-3.97,1.175,0.04));
#21983=CARTESIAN_POINT('',(-3.97,1.175,0.4));
#21984=CARTESIAN_POINT('',(-3.43500000000001,1.71,0.574999999999998));
#21985=CARTESIAN_POINT('Origin',(0.,-3.14975114354414E-17,1.9893933982822));
#21986=CARTESIAN_POINT('',(-1.0287867965644,2.46519032881566E-32,1.9787867965644));
#21987=CARTESIAN_POINT('Origin',(0.,-6.29950228708828E-17,1.9787867965644));
#21988=CARTESIAN_POINT('',(-1.08,-1.32261854307914E-16,2.));
#21989=CARTESIAN_POINT('',(-1.0543933982822,6.61309271539571E-17,1.9893933982822));
#21990=CARTESIAN_POINT('Origin',(0.,0.,2.));
#21991=CARTESIAN_POINT('Origin',(0.,0.,1.975));
#21992=CARTESIAN_POINT('',(-1.0212132034356,-2.50125096166884E-16,1.9712132034356));
#21993=CARTESIAN_POINT('',(-1.025,-1.25526296912604E-16,1.975));
#21994=CARTESIAN_POINT('Origin',(0.,-6.25312740417209E-17,1.9712132034356));
#21995=CARTESIAN_POINT('Origin',(0.,0.,2.));
#21996=CARTESIAN_POINT('',(-1.54,1.88595607068692E-16,2.));
#21997=CARTESIAN_POINT('Origin',(0.,0.,2.));
#21998=CARTESIAN_POINT('Origin',(0.,-3.12656370208604E-17,1.9456066017178));
#21999=CARTESIAN_POINT('',(-1.,1.22464679914735E-16,1.92));
#22000=CARTESIAN_POINT('',(-1.0106066017178,-1.86294888040809E-16,1.9456066017178));
#22001=CARTESIAN_POINT('Origin',(0.,0.,1.92));
#22002=CARTESIAN_POINT('Origin',(0.,0.,2.));
#22003=CARTESIAN_POINT('',(-1.,-1.22464679914735E-16,0.4));
#22004=CARTESIAN_POINT('',(-1.,1.22464679914735E-16,2.));
#22005=CARTESIAN_POINT('Origin',(0.,0.,0.4));
#22006=CARTESIAN_POINT('',(0.234267305685713,0.972172222132867,1.4));
#22007=CARTESIAN_POINT('Ctrl Pts',(0.234267305685713,0.972172222132867,
1.4));
#22008=CARTESIAN_POINT('Ctrl Pts',(0.234267305685713,0.972172222132867,
1.43391900663149));
#22009=CARTESIAN_POINT('Ctrl Pts',(0.217453199576997,0.97640750358249,1.50750370302361));
#22010=CARTESIAN_POINT('Ctrl Pts',(0.162557143889187,0.987394406811514,
1.57537359399088));
#22011=CARTESIAN_POINT('Ctrl Pts',(0.103338063857534,0.99504750544363,1.61334001682052));
#22012=CARTESIAN_POINT('Ctrl Pts',(0.0342814671797575,1.00049861473999,
1.63725191259632));
#22013=CARTESIAN_POINT('Ctrl Pts',(-0.0343654764701675,1.00042505413025,
1.63680882232891));
#22014=CARTESIAN_POINT('Ctrl Pts',(-0.103211592970685,0.995066437220061,
1.61345114045812));
#22015=CARTESIAN_POINT('Ctrl Pts',(-0.148329808958505,0.989169324847084,
1.58415597304455));
#22016=CARTESIAN_POINT('Ctrl Pts',(-0.183849662047555,0.983122988023421,
1.54896583267799));
#22017=CARTESIAN_POINT('Ctrl Pts',(-0.222528948857546,0.975130828482948,
1.48743715896112));
#22018=CARTESIAN_POINT('Ctrl Pts',(-0.242031304986677,0.970123636918925,
1.40006630054004));
#22019=CARTESIAN_POINT('Ctrl Pts',(-0.222407063698446,0.975220619502292,
1.31224680544824));
#22020=CARTESIAN_POINT('Ctrl Pts',(-0.183657702453494,0.983122398337006,
1.25122736917816));
#22021=CARTESIAN_POINT('Ctrl Pts',(-0.13684634930182,0.991308187330295,
1.20344105854914));
#22022=CARTESIAN_POINT('Ctrl Pts',(-0.0520840197900239,1.0005765283454,
1.16234073969225));
#22023=CARTESIAN_POINT('Ctrl Pts',(0.0343068301640742,1.00047914632208,
1.16292703932357));
#22024=CARTESIAN_POINT('Ctrl Pts',(0.10329410020646,0.995062702176677,1.18658091767974));
#22025=CARTESIAN_POINT('Ctrl Pts',(0.162577481379246,0.987395818375031,
1.22465007697402));
#22026=CARTESIAN_POINT('Ctrl Pts',(0.217435775063741,0.97641259628012,1.29246754064607));
#22027=CARTESIAN_POINT('Ctrl Pts',(0.234267305685713,0.972172222132867,
1.36608099336852));
#22028=CARTESIAN_POINT('Ctrl Pts',(0.234267305685713,0.972172222132867,
1.4));
#22029=CARTESIAN_POINT('Ctrl Pts',(0.234267305685713,0.972172222132867,
1.4));
#22030=CARTESIAN_POINT('Ctrl Pts',(0.234267305685713,0.972172222132867,
1.36608099336852));
#22031=CARTESIAN_POINT('Ctrl Pts',(0.217435775063741,0.97641259628012,1.29246754064607));
#22032=CARTESIAN_POINT('Ctrl Pts',(0.162577481379246,0.987395818375031,
1.22465007697402));
#22033=CARTESIAN_POINT('Ctrl Pts',(0.10329410020646,0.995062702176677,1.18658091767974));
#22034=CARTESIAN_POINT('Ctrl Pts',(0.0343068301640742,1.00047914632208,
1.16292703932357));
#22035=CARTESIAN_POINT('Ctrl Pts',(-0.0520840197900239,1.0005765283454,
1.16234073969225));
#22036=CARTESIAN_POINT('Ctrl Pts',(-0.13684634930182,0.991308187330295,
1.20344105854914));
#22037=CARTESIAN_POINT('Ctrl Pts',(-0.183657702453494,0.983122398337006,
1.25122736917816));
#22038=CARTESIAN_POINT('Ctrl Pts',(-0.222407063698446,0.975220619502292,
1.31224680544824));
#22039=CARTESIAN_POINT('Ctrl Pts',(-0.242031304986677,0.970123636918925,
1.40006630054004));
#22040=CARTESIAN_POINT('Ctrl Pts',(-0.222528948857546,0.975130828482948,
1.48743715896112));
#22041=CARTESIAN_POINT('Ctrl Pts',(-0.183849662047555,0.983122988023421,
1.54896583267799));
#22042=CARTESIAN_POINT('Ctrl Pts',(-0.148329808958505,0.989169324847084,
1.58415597304455));
#22043=CARTESIAN_POINT('Ctrl Pts',(-0.103211592970685,0.995066437220061,
1.61345114045812));
#22044=CARTESIAN_POINT('Ctrl Pts',(-0.0343654764701675,1.00042505413025,
1.63680882232891));
#22045=CARTESIAN_POINT('Ctrl Pts',(0.0342814671797575,1.00049861473999,
1.63725191259632));
#22046=CARTESIAN_POINT('Ctrl Pts',(0.103338063857534,0.99504750544363,1.61334001682052));
#22047=CARTESIAN_POINT('Ctrl Pts',(0.162557143889187,0.987394406811514,
1.57537359399088));
#22048=CARTESIAN_POINT('Ctrl Pts',(0.217453199576997,0.97640750358249,1.50750370302361));
#22049=CARTESIAN_POINT('Ctrl Pts',(0.234267305685713,0.972172222132867,
1.43391900663149));
#22050=CARTESIAN_POINT('Ctrl Pts',(0.234267305685713,0.972172222132867,
1.4));
#22051=CARTESIAN_POINT('Ctrl Pts',(0.224511537123809,0.984368805790859,
1.4));
#22052=CARTESIAN_POINT('Ctrl Pts',(0.224511537123809,0.984368805790859,
1.36785293603036));
#22053=CARTESIAN_POINT('Ctrl Pts',(0.208715983620224,0.988232116107654,
1.29804318701526));
#22054=CARTESIAN_POINT('Ctrl Pts',(0.156597374287794,0.998329294088653,
1.23289572937968));
#22055=CARTESIAN_POINT('Ctrl Pts',(0.0996850231726542,1.00542138378364,
1.19601708761738));
#22056=CARTESIAN_POINT('Ctrl Pts',(0.0331933469447592,1.01044296116397,
1.17298582817999));
#22057=CARTESIAN_POINT('Ctrl Pts',(-0.0504018911245414,1.01053249517299,
1.17242112850164));
#22058=CARTESIAN_POINT('Ctrl Pts',(-0.131966316236839,1.00194232959414,
1.21241761585945));
#22059=CARTESIAN_POINT('Ctrl Pts',(-0.176623835810546,0.994399145207215,
1.25842866128864));
#22060=CARTESIAN_POINT('Ctrl Pts',(-0.21338883997175,0.987146498650659,
1.31681134873593));
#22061=CARTESIAN_POINT('Ctrl Pts',(-0.231784665389821,0.982502518259946,
1.40006723250035));
#22062=CARTESIAN_POINT('Ctrl Pts',(-0.213493242367903,0.987065442519242,
1.48288286604478));
#22063=CARTESIAN_POINT('Ctrl Pts',(-0.176810077065311,0.994399827877688,
1.54175634937481));
#22064=CARTESIAN_POINT('Ctrl Pts',(-0.142905163319919,0.999972627766867,
1.5756422556539));
#22065=CARTESIAN_POINT('Ctrl Pts',(-0.099608650549313,1.00542488505706,
1.60401383731078));
#22066=CARTESIAN_POINT('Ctrl Pts',(-0.03323883765608,1.01039449521007,1.62676344662667));
#22067=CARTESIAN_POINT('Ctrl Pts',(0.033164982119191,1.01046069537358,1.62718522868402));
#22068=CARTESIAN_POINT('Ctrl Pts',(0.0997312542373632,1.00540762238061,
1.60390736404938));
#22069=CARTESIAN_POINT('Ctrl Pts',(0.156576887349813,0.998328050935301,
1.56712687096736));
#22070=CARTESIAN_POINT('Ctrl Pts',(0.208734202187127,0.988227502023521,
1.50192933822754));
#22071=CARTESIAN_POINT('Ctrl Pts',(0.224511537123809,0.984368805790859,
1.43214706396964));
#22072=CARTESIAN_POINT('Ctrl Pts',(0.224511537123809,0.984368805790859,
1.4));
#22073=CARTESIAN_POINT('Ctrl Pts',(0.214755768561905,0.996565389448851,
1.4));
#22074=CARTESIAN_POINT('Ctrl Pts',(0.214755768561905,0.996565389448851,
1.36962487869221));
#22075=CARTESIAN_POINT('Ctrl Pts',(0.199996192176708,1.00005163593519,1.30361883338444));
#22076=CARTESIAN_POINT('Ctrl Pts',(0.150617267196342,1.00926276980227,1.24114138178534));
#22077=CARTESIAN_POINT('Ctrl Pts',(0.096075946138849,1.01578006539061,1.20545325755502));
#22078=CARTESIAN_POINT('Ctrl Pts',(0.0320798637254439,1.02040677600585,
1.18304461703641));
#22079=CARTESIAN_POINT('Ctrl Pts',(-0.0487197624590589,1.02048846200059,
1.18250151731103));
#22080=CARTESIAN_POINT('Ctrl Pts',(-0.127086283171857,1.01257647185799,
1.22139417316976));
#22081=CARTESIAN_POINT('Ctrl Pts',(-0.169589969167599,1.00567589207742,
1.26562995339912));
#22082=CARTESIAN_POINT('Ctrl Pts',(-0.204370616245054,0.999072377799025,
1.32137589202362));
#22083=CARTESIAN_POINT('Ctrl Pts',(-0.221538025792965,0.994881399600966,
1.40006816446067));
#22084=CARTESIAN_POINT('Ctrl Pts',(-0.20445753587826,0.999000056555535,
1.47832857312844));
#22085=CARTESIAN_POINT('Ctrl Pts',(-0.169770492083067,1.00567666773195,
1.53454686607163));
#22086=CARTESIAN_POINT('Ctrl Pts',(-0.137480517681333,1.01077593068665,
1.56712853826326));
#22087=CARTESIAN_POINT('Ctrl Pts',(-0.0960057081279411,1.01578333289406,
1.59457653416343));
#22088=CARTESIAN_POINT('Ctrl Pts',(-0.0321121988419924,1.02036393628989,
1.61671807092442));
#22089=CARTESIAN_POINT('Ctrl Pts',(0.0320484970586246,1.02042277600718,
1.61711854477173));
#22090=CARTESIAN_POINT('Ctrl Pts',(0.0961244446171922,1.01576773931759,
1.59447471127824));
#22091=CARTESIAN_POINT('Ctrl Pts',(0.150596630810439,1.00926169505909,1.55888014794385));
#22092=CARTESIAN_POINT('Ctrl Pts',(0.200015204797257,1.00004750046455,1.49635497343148));
#22093=CARTESIAN_POINT('Ctrl Pts',(0.214755768561905,0.996565389448851,
1.43037512130779));
#22094=CARTESIAN_POINT('Ctrl Pts',(0.214755768561905,0.996565389448851,
1.4));
#22095=CARTESIAN_POINT('Ctrl Pts',(0.205,1.00876197310684,1.4));
#22096=CARTESIAN_POINT('Ctrl Pts',(0.205,1.00876197310684,1.37139682135405));
#22097=CARTESIAN_POINT('Ctrl Pts',(0.191276400733191,1.01187115576272,1.30919447975363));
#22098=CARTESIAN_POINT('Ctrl Pts',(0.14463716010489,1.0201962455159,1.249387034191));
#22099=CARTESIAN_POINT('Ctrl Pts',(0.0924668691050436,1.02613874699757,
1.21488942749266));
#22100=CARTESIAN_POINT('Ctrl Pts',(0.0309663805061289,1.03037059084774,
1.19310340589283));
#22101=CARTESIAN_POINT('Ctrl Pts',(-0.0470376337935765,1.03044442882818,
1.19258190612042));
#22102=CARTESIAN_POINT('Ctrl Pts',(-0.122206250106876,1.02321061412184,
1.23037073048007));
#22103=CARTESIAN_POINT('Ctrl Pts',(-0.162556102524651,1.01695263894763,
1.2728312455096));
#22104=CARTESIAN_POINT('Ctrl Pts',(-0.195352392518359,1.01099825694739,
1.3259404353113));
#22105=CARTESIAN_POINT('Ctrl Pts',(-0.211291386196109,1.00726028094199,
1.40006909642098));
#22106=CARTESIAN_POINT('Ctrl Pts',(-0.195421829388617,1.01093467059183,
1.47377428021209));
#22107=CARTESIAN_POINT('Ctrl Pts',(-0.162730907100823,1.01695350758622,
1.52733738276844));
#22108=CARTESIAN_POINT('Ctrl Pts',(-0.132055872042747,1.02157923360643,
1.55861482087262));
#22109=CARTESIAN_POINT('Ctrl Pts',(-0.0924027657065692,1.02614178073107,
1.58513923101609));
#22110=CARTESIAN_POINT('Ctrl Pts',(-0.0309855600279049,1.03033337736971,
1.60667269522218));
#22111=CARTESIAN_POINT('Ctrl Pts',(0.0309320119980581,1.03038485664077,
1.60705186085944));
#22112=CARTESIAN_POINT('Ctrl Pts',(0.0925176349970211,1.02612785625456,
1.58504205850711));
#22113=CARTESIAN_POINT('Ctrl Pts',(0.144616374271065,1.02019533918288,1.55063342492034));
#22114=CARTESIAN_POINT('Ctrl Pts',(0.191296207407388,1.01186749890558,1.49078060863542));
#22115=CARTESIAN_POINT('Ctrl Pts',(0.205,1.00876197310684,1.42860317864595));
#22116=CARTESIAN_POINT('Ctrl Pts',(0.205,1.00876197310684,1.4));
#22117=CARTESIAN_POINT('',(0.205,1.00876197310684,1.4));
#22118=CARTESIAN_POINT('',(0.234267305685713,0.972172222132867,1.4));
#22119=CARTESIAN_POINT('',(-0.000185900815659297,1.03004010593546,1.19476336551356));
#22120=CARTESIAN_POINT('Ctrl Pts',(0.205,1.00876197310684,1.4));
#22121=CARTESIAN_POINT('Ctrl Pts',(0.205,1.00876197310684,1.37139682135405));
#22122=CARTESIAN_POINT('Ctrl Pts',(0.191276400733191,1.01187115576272,1.30919447975363));
#22123=CARTESIAN_POINT('Ctrl Pts',(0.14463716010489,1.0201962455159,1.249387034191));
#22124=CARTESIAN_POINT('Ctrl Pts',(0.0924668691050436,1.02613874699757,
1.21488942749266));
#22125=CARTESIAN_POINT('Ctrl Pts',(0.0463415026558576,1.0293126298852,1.19854991129279));
#22126=CARTESIAN_POINT('Ctrl Pts',(0.0152903507427837,1.03003762732168,
1.19477984108684));
#22127=CARTESIAN_POINT('Ctrl Pts',(-0.000201953715795163,1.03004356916167,
1.19474293166142));
#22128=CARTESIAN_POINT('Ctrl Pts',(-0.000201953715795163,1.03004356916167,
1.19474293166142));
#22129=CARTESIAN_POINT('Ctrl Pts',(-0.015694258174374,1.03004951100166,
1.19470602223599));
#22130=CARTESIAN_POINT('Ctrl Pts',(-0.0620713570562364,1.02899766588691,
1.20013967099235));
#22131=CARTESIAN_POINT('Ctrl Pts',(-0.122206250106876,1.02321061412184,
1.23037073048007));
#22132=CARTESIAN_POINT('Ctrl Pts',(-0.162556102524651,1.01695263894763,
1.2728312455096));
#22133=CARTESIAN_POINT('Ctrl Pts',(-0.195352392518359,1.01099825694739,
1.3259404353113));
#22134=CARTESIAN_POINT('Ctrl Pts',(-0.211291386196109,1.00726028094199,
1.40006909642098));
#22135=CARTESIAN_POINT('Ctrl Pts',(-0.195421829388617,1.01093467059183,
1.47377428021209));
#22136=CARTESIAN_POINT('Ctrl Pts',(-0.162730907100823,1.01695350758622,
1.52733738276844));
#22137=CARTESIAN_POINT('Ctrl Pts',(-0.132055872042747,1.02157923360643,
1.55861482087262));
#22138=CARTESIAN_POINT('Ctrl Pts',(-0.0924027657065692,1.02614178073107,
1.58513923101609));
#22139=CARTESIAN_POINT('Ctrl Pts',(-0.0309855600279049,1.03033337736971,
1.60667269522218));
#22140=CARTESIAN_POINT('Ctrl Pts',(0.0309320119980581,1.03038485664077,
1.60705186085944));
#22141=CARTESIAN_POINT('Ctrl Pts',(0.0925176349970211,1.02612785625456,
1.58504205850711));
#22142=CARTESIAN_POINT('Ctrl Pts',(0.144616374271065,1.02019533918288,1.55063342492034));
#22143=CARTESIAN_POINT('Ctrl Pts',(0.191296207407388,1.01186749890558,1.49078060863542));
#22144=CARTESIAN_POINT('Ctrl Pts',(0.205,1.00876197310684,1.42860317864595));
#22145=CARTESIAN_POINT('Ctrl Pts',(0.205,1.00876197310684,1.4));
#22146=CARTESIAN_POINT('Origin',(0.,1.3,1.4));
#22147=CARTESIAN_POINT('',(0.000131092032552791,1.57001173019275,1.19489555472783));
#22148=CARTESIAN_POINT('',(-2.51052593825207E-17,1.3,1.195));
#22149=CARTESIAN_POINT('',(-0.205,1.55681284340656,1.4));
#22150=CARTESIAN_POINT('Ctrl Pts',(-0.205,1.55681284340656,1.4));
#22151=CARTESIAN_POINT('Ctrl Pts',(-0.205,1.55681284340656,1.36999095977411));
#22152=CARTESIAN_POINT('Ctrl Pts',(-0.189388171591284,1.55880764860196,
1.30517776395932));
#22153=CARTESIAN_POINT('Ctrl Pts',(-0.131226834866621,1.56517193552246,
1.23336580368775));
#22154=CARTESIAN_POINT('Ctrl Pts',(-0.0588701281878798,1.56936404629955,
1.19995504443905));
#22155=CARTESIAN_POINT('Ctrl Pts',(-0.0146362597178014,1.5700109088422,
1.19488207104102));
#22156=CARTESIAN_POINT('Ctrl Pts',(0.000131092032552795,1.57001173019275,
1.19489555472783));
#22157=CARTESIAN_POINT('Ctrl Pts',(0.000131092032552795,1.57001173019275,
1.19489555472783));
#22158=CARTESIAN_POINT('Ctrl Pts',(0.014898443782907,1.57001255154331,1.19490903841464));
#22159=CARTESIAN_POINT('Ctrl Pts',(0.0592686858149541,1.56937061710401,
1.20006291393354));
#22160=CARTESIAN_POINT('Ctrl Pts',(0.11788137682178,1.56585072182196,1.22787750075822));
#22161=CARTESIAN_POINT('Ctrl Pts',(0.15953730265344,1.56201454198299,1.26923760937899));
#22162=CARTESIAN_POINT('Ctrl Pts',(0.211865794877702,1.55611977186479,1.34957830861567));
#22163=CARTESIAN_POINT('Ctrl Pts',(0.211750431534509,1.55626070984013,1.45021602420942));
#22164=CARTESIAN_POINT('Ctrl Pts',(0.159496444970874,1.56209212184905,1.53092039588429));
#22165=CARTESIAN_POINT('Ctrl Pts',(0.117816060861919,1.56594151821204,1.57228130294414));
#22166=CARTESIAN_POINT('Ctrl Pts',(0.0442687531132715,1.57029071330042,
1.60696014729065));
#22167=CARTESIAN_POINT('Ctrl Pts',(-0.0441540900742972,1.57022524422482,
1.60664163567999));
#22168=CARTESIAN_POINT('Ctrl Pts',(-0.131461869516863,1.56518094711964,
1.56655738881618));
#22169=CARTESIAN_POINT('Ctrl Pts',(-0.189333853997008,1.55881441935392,
1.49480011859911));
#22170=CARTESIAN_POINT('Ctrl Pts',(-0.205,1.55681284340656,1.43000904022589));
#22171=CARTESIAN_POINT('Ctrl Pts',(-0.205,1.55681284340656,1.4));
#22172=CARTESIAN_POINT('Origin',(3.985,1.84,0.4));
#22173=CARTESIAN_POINT('',(3.985,1.84,0.0250000000000001));
#22174=CARTESIAN_POINT('',(4.,1.855,0.04));
#22175=CARTESIAN_POINT('',(3.48916666666666,1.34416666666665,-0.470833333333338));
#22176=CARTESIAN_POINT('',(4.,1.855,0.71));
#22177=CARTESIAN_POINT('',(4.,1.855,0.4));
#22178=CARTESIAN_POINT('',(3.98242640687119,1.83742640687119,0.752426406871192));
#22179=CARTESIAN_POINT('',(3.77907310450642,1.63407310450642,1.24336470739356));
#22180=CARTESIAN_POINT('',(3.97,1.825,0.74));
#22181=CARTESIAN_POINT('',(3.44166666666668,1.29666666666667,0.21166666666667));
#22182=CARTESIAN_POINT('',(3.97,1.825,0.04));
#22183=CARTESIAN_POINT('',(3.97,1.825,0.4));
#22184=CARTESIAN_POINT('',(3.43500000000002,1.29,0.574999999999997));
#22185=CARTESIAN_POINT('Origin',(2.1,1.825,0.8));
#22186=CARTESIAN_POINT('',(2.1,1.825,0.74));
#22187=CARTESIAN_POINT('',(1.05,1.825,0.74));
#22188=CARTESIAN_POINT('',(2.1,1.825,0.04));
#22189=CARTESIAN_POINT('',(2.1,1.825,0.8));
#22190=CARTESIAN_POINT('',(1.05,1.825,0.04));
#22191=CARTESIAN_POINT('Origin',(1.05,1.855,0.77));
#22192=CARTESIAN_POINT('',(3.9787867965644,1.8462132034356,0.761213203435596));
#22193=CARTESIAN_POINT('',(4.25493545624507,1.17953136400341,0.094531364003406));
#22194=CARTESIAN_POINT('',(3.9612132034356,1.8637867965644,0.778786796564404));
#22195=CARTESIAN_POINT('',(3.94,1.885,0.8));
#22196=CARTESIAN_POINT('',(2.1,1.8637867965644,0.778786796564404));
#22197=CARTESIAN_POINT('',(0.525,1.8637867965644,0.778786796564404));
#22198=CARTESIAN_POINT('',(2.1,1.825,0.74));
#22199=CARTESIAN_POINT('Origin',(3.9893933982822,-2.25,0.735606601717798));
#22200=CARTESIAN_POINT('',(4.,2.6,0.71));
#22201=CARTESIAN_POINT('',(4.,-2.25,0.71));
#22202=CARTESIAN_POINT('',(3.9787867965644,2.6,0.761213203435597));
#22203=CARTESIAN_POINT('',(4.,2.6,0.71));
#22204=CARTESIAN_POINT('',(3.9787867965644,-2.25,0.761213203435596));
#22205=CARTESIAN_POINT('Origin',(-3.985,1.84,0.4));
#22206=CARTESIAN_POINT('',(-3.98242640687119,1.83742640687119,0.752426406871192));
#22207=CARTESIAN_POINT('',(-4.,1.855,0.71));
#22208=CARTESIAN_POINT('',(-4.06648716152533,1.92148716152533,0.549485792921871));
#22209=CARTESIAN_POINT('',(-4.,1.855,0.04));
#22210=CARTESIAN_POINT('',(-4.,1.855,0.4));
#22211=CARTESIAN_POINT('',(-3.985,1.84,0.0250000000000002));
#22212=CARTESIAN_POINT('',(-3.98916666666666,1.84416666666666,0.029166666666665));
#22213=CARTESIAN_POINT('',(-3.97,1.825,0.04));
#22214=CARTESIAN_POINT('',(-3.60166666666668,1.45666666666667,0.408333333333331));
#22215=CARTESIAN_POINT('',(-3.97,1.825,0.74));
#22216=CARTESIAN_POINT('',(-3.97,1.825,0.4));
#22217=CARTESIAN_POINT('',(-3.60833333333335,1.46333333333334,0.378333333333335));
#22218=CARTESIAN_POINT('Origin',(-3.98,1.5,0.02));
#22219=CARTESIAN_POINT('',(-4.,2.6,0.04));
#22220=CARTESIAN_POINT('',(-4.,1.5,0.04));
#22221=CARTESIAN_POINT('',(-3.96,2.6,0.));
#22222=CARTESIAN_POINT('',(-3.96,2.6,0.));
#22223=CARTESIAN_POINT('',(-3.96,1.865,0.));
#22224=CARTESIAN_POINT('',(-3.96,1.5,0.));
#22225=CARTESIAN_POINT('',(-3.96,1.865,0.));
#22226=CARTESIAN_POINT('Origin',(-4.,3.,0.));
#22227=CARTESIAN_POINT('',(-4.,2.6,0.71));
#22228=CARTESIAN_POINT('',(-4.,2.25,0.71));
#22229=CARTESIAN_POINT('',(-4.,2.6,0.));
#22230=CARTESIAN_POINT('Origin',(-3.9893933982822,2.25,0.735606601717798));
#22231=CARTESIAN_POINT('',(-3.9787867965644,1.8462132034356,0.761213203435597));
#22232=CARTESIAN_POINT('',(-3.86526671090596,2.12027493383395,1.03527493383395));
#22233=CARTESIAN_POINT('',(-3.9787867965644,2.6,0.761213203435597));
#22234=CARTESIAN_POINT('',(-3.9787867965644,2.25,0.761213203435596));
#22235=CARTESIAN_POINT('',(-4.,2.6,0.71));
#22236=CARTESIAN_POINT('Origin',(3.6,2.6,0.735606601717798));
#22237=CARTESIAN_POINT('',(3.6,3.,0.71));
#22238=CARTESIAN_POINT('',(3.6,2.9787867965644,0.761213203435597));
#22239=CARTESIAN_POINT('',(3.6,3.,0.71));
#22240=CARTESIAN_POINT('Origin',(3.6,2.6,0.761213203435597));
#22241=CARTESIAN_POINT('Origin',(3.6,2.6,0.71));
#22242=CARTESIAN_POINT('Origin',(3.,2.9893933982822,0.735606601717798));
#22243=CARTESIAN_POINT('',(-3.6,3.,0.71));
#22244=CARTESIAN_POINT('',(-3.6,2.9787867965644,0.761213203435597));
#22245=CARTESIAN_POINT('',(-3.6,3.,0.71));
#22246=CARTESIAN_POINT('',(3.,2.9787867965644,0.761213203435596));
#22247=CARTESIAN_POINT('',(3.,3.,0.71));
#22248=CARTESIAN_POINT('Origin',(-3.6,2.6,0.735606601717798));
#22249=CARTESIAN_POINT('Origin',(-3.6,2.6,0.761213203435597));
#22250=CARTESIAN_POINT('Origin',(-3.6,2.6,0.71));
#22251=CARTESIAN_POINT('Origin',(-2.05,1.855,0.77));
#22252=CARTESIAN_POINT('',(-2.1,1.825,0.74));
#22253=CARTESIAN_POINT('',(-2.05,1.825,0.74));
#22254=CARTESIAN_POINT('',(-2.1,1.8637867965644,0.778786796564404));
#22255=CARTESIAN_POINT('',(-2.1,1.825,0.74));
#22256=CARTESIAN_POINT('',(-3.9612132034356,1.8637867965644,0.778786796564404));
#22257=CARTESIAN_POINT('',(-1.025,1.8637867965644,0.778786796564404));
#22258=CARTESIAN_POINT('',(-3.94,1.885,0.8));
#22259=CARTESIAN_POINT('Origin',(-4.1,1.825,0.8));
#22260=CARTESIAN_POINT('',(-2.1,1.825,0.04));
#22261=CARTESIAN_POINT('',(-2.05,1.825,0.04));
#22262=CARTESIAN_POINT('',(-2.1,1.825,0.8));
#22263=CARTESIAN_POINT('Origin',(-3.6,2.6,0.));
#22264=CARTESIAN_POINT('',(-3.6,3.,0.04));
#22265=CARTESIAN_POINT('',(-3.6,3.,0.));
#22266=CARTESIAN_POINT('Origin',(-3.6,2.6,0.04));
#22267=CARTESIAN_POINT('Origin',(4.,3.,0.));
#22268=CARTESIAN_POINT('',(3.6,3.,0.04));
#22269=CARTESIAN_POINT('',(3.6,3.,0.));
#22270=CARTESIAN_POINT('',(2.,3.,0.04));
#22271=CARTESIAN_POINT('Origin',(3.6,2.6,0.));
#22272=CARTESIAN_POINT('',(4.,2.6,0.04));
#22273=CARTESIAN_POINT('',(4.,2.6,0.));
#22274=CARTESIAN_POINT('Origin',(3.6,2.6,0.04));
#22275=CARTESIAN_POINT('Origin',(4.,-3.,0.));
#22276=CARTESIAN_POINT('',(4.,-1.5,0.04));
#22277=CARTESIAN_POINT('Origin',(-3.9356066017178,0.75,0.789393398282202));
#22278=CARTESIAN_POINT('',(-3.91,1.915,0.8));
#22279=CARTESIAN_POINT('',(-3.52778855802712,2.29721144197289,0.958317162959347));
#22280=CARTESIAN_POINT('',(-3.91,2.6,0.8));
#22281=CARTESIAN_POINT('',(-3.91,0.75,0.8));
#22282=CARTESIAN_POINT('',(-3.9612132034356,2.6,0.778786796564403));
#22283=CARTESIAN_POINT('',(-3.91,2.6,0.8));
#22284=CARTESIAN_POINT('',(-3.9612132034356,0.75,0.778786796564403));
#22285=CARTESIAN_POINT('Origin',(-3.6,2.6,0.789393398282202));
#22286=CARTESIAN_POINT('',(-3.6,2.91,0.8));
#22287=CARTESIAN_POINT('',(-3.6,2.9612132034356,0.778786796564404));
#22288=CARTESIAN_POINT('',(-3.6,2.91,0.8));
#22289=CARTESIAN_POINT('Origin',(-3.6,2.6,0.778786796564404));
#22290=CARTESIAN_POINT('Origin',(-3.6,2.6,0.8));
#22291=CARTESIAN_POINT('Origin',(1.,2.9356066017178,0.789393398282202));
#22292=CARTESIAN_POINT('',(3.6,2.91,0.8));
#22293=CARTESIAN_POINT('',(3.6,2.9612132034356,0.778786796564403));
#22294=CARTESIAN_POINT('',(3.6,2.91,0.8));
#22295=CARTESIAN_POINT('',(1.,2.9612132034356,0.778786796564403));
#22296=CARTESIAN_POINT('',(1.,2.91,0.8));
#22297=CARTESIAN_POINT('Origin',(3.6,2.6,0.789393398282202));
#22298=CARTESIAN_POINT('',(3.91,2.6,0.8));
#22299=CARTESIAN_POINT('',(3.9612132034356,2.6,0.778786796564404));
#22300=CARTESIAN_POINT('',(3.91,2.6,0.8));
#22301=CARTESIAN_POINT('Origin',(3.6,2.6,0.778786796564404));
#22302=CARTESIAN_POINT('Origin',(3.6,2.6,0.8));
#22303=CARTESIAN_POINT('Origin',(3.9356066017178,-0.75,0.789393398282202));
#22304=CARTESIAN_POINT('',(3.91,1.915,0.8));
#22305=CARTESIAN_POINT('',(3.75803641463731,2.0669635853627,0.86294537804407));
#22306=CARTESIAN_POINT('',(3.9612132034356,-0.75,0.778786796564403));
#22307=CARTESIAN_POINT('',(3.91,-0.75,0.8));
#22308=CARTESIAN_POINT('Origin',(-3.97,1.5,0.77));
#22309=CARTESIAN_POINT('',(-4.,2.6,0.74));
#22310=CARTESIAN_POINT('Origin',(-3.6,2.6,0.77));
#22311=CARTESIAN_POINT('',(-3.6,3.,0.74));
#22312=CARTESIAN_POINT('Origin',(2.,2.97,0.77));
#22313=CARTESIAN_POINT('',(3.6,3.,0.74));
#22314=CARTESIAN_POINT('Origin',(3.6,2.6,0.77));
#22315=CARTESIAN_POINT('',(4.,2.6,0.74));
#22316=CARTESIAN_POINT('Origin',(3.97,-1.5,0.77));
#22317=CARTESIAN_POINT('Origin',(0.525,1.8893933982822,0.789393398282202));
#22318=CARTESIAN_POINT('',(2.1,1.915,0.8));
#22319=CARTESIAN_POINT('',(0.525,1.915,0.8));
#22320=CARTESIAN_POINT('',(2.1,1.915,0.8));
#22321=CARTESIAN_POINT('Origin',(2.1,1.5,0.789393398282202));
#22322=CARTESIAN_POINT('',(2.1,1.085,0.8));
#22323=CARTESIAN_POINT('',(2.1,1.085,0.8));
#22324=CARTESIAN_POINT('Origin',(2.1,1.5,0.778786796564404));
#22325=CARTESIAN_POINT('Origin',(2.1,1.5,0.8));
#22326=CARTESIAN_POINT('Origin',(1.025,1.1106066017178,0.789393398282202));
#22327=CARTESIAN_POINT('',(3.91,1.085,0.8));
#22328=CARTESIAN_POINT('',(1.025,1.085,0.8));
#22329=CARTESIAN_POINT('',(3.91,1.085,0.8));
#22330=CARTESIAN_POINT('Origin',(3.9356066017178,-0.75,0.789393398282202));
#22331=CARTESIAN_POINT('',(3.91,-1.085,0.8));
#22332=CARTESIAN_POINT('',(3.91,-0.75,0.8));
#22333=CARTESIAN_POINT('',(3.91,-1.085,0.8));
#22334=CARTESIAN_POINT('Origin',(0.525,-1.1106066017178,0.789393398282202));
#22335=CARTESIAN_POINT('',(2.1,-1.085,0.8));
#22336=CARTESIAN_POINT('',(0.525,-1.085,0.8));
#22337=CARTESIAN_POINT('',(2.1,-1.085,0.8));
#22338=CARTESIAN_POINT('Origin',(2.1,-1.5,0.789393398282202));
#22339=CARTESIAN_POINT('',(2.1,-1.915,0.8));
#22340=CARTESIAN_POINT('',(2.1,-1.915,0.8));
#22341=CARTESIAN_POINT('Origin',(2.1,-1.5,0.778786796564404));
#22342=CARTESIAN_POINT('Origin',(2.1,-1.5,0.8));
#22343=CARTESIAN_POINT('Origin',(1.025,-1.8893933982822,0.789393398282202));
#22344=CARTESIAN_POINT('',(3.91,-1.915,0.8));
#22345=CARTESIAN_POINT('',(1.025,-1.915,0.8));
#22346=CARTESIAN_POINT('',(3.91,-1.915,0.8));
#22347=CARTESIAN_POINT('Origin',(3.9356066017178,-0.75,0.789393398282202));
#22348=CARTESIAN_POINT('',(3.91,-2.6,0.8));
#22349=CARTESIAN_POINT('',(3.91,-0.75,0.8));
#22350=CARTESIAN_POINT('',(3.91,-2.6,0.8));
#22351=CARTESIAN_POINT('Origin',(3.6,-2.6,0.789393398282202));
#22352=CARTESIAN_POINT('',(3.6,-2.91,0.8));
#22353=CARTESIAN_POINT('',(3.6,-2.9612132034356,0.778786796564404));
#22354=CARTESIAN_POINT('',(3.6,-2.91,0.8));
#22355=CARTESIAN_POINT('Origin',(3.6,-2.6,0.778786796564404));
#22356=CARTESIAN_POINT('Origin',(3.6,-2.6,0.8));
#22357=CARTESIAN_POINT('Origin',(-1.,-2.9356066017178,0.789393398282202));
#22358=CARTESIAN_POINT('',(-3.6,-2.91,0.8));
#22359=CARTESIAN_POINT('',(-3.6,-2.9612132034356,0.778786796564403));
#22360=CARTESIAN_POINT('',(-3.6,-2.91,0.8));
#22361=CARTESIAN_POINT('',(-1.,-2.9612132034356,0.778786796564403));
#22362=CARTESIAN_POINT('',(-1.,-2.91,0.8));
#22363=CARTESIAN_POINT('Origin',(-3.6,-2.6,0.789393398282202));
#22364=CARTESIAN_POINT('',(-3.91,-2.6,0.8));
#22365=CARTESIAN_POINT('',(-3.91,-2.6,0.8));
#22366=CARTESIAN_POINT('Origin',(-3.6,-2.6,0.778786796564404));
#22367=CARTESIAN_POINT('Origin',(-3.6,-2.6,0.8));
#22368=CARTESIAN_POINT('Origin',(-3.9356066017178,0.75,0.789393398282202));
#22369=CARTESIAN_POINT('',(-3.91,-1.915,0.8));
#22370=CARTESIAN_POINT('',(-3.91,0.75,0.8));
#22371=CARTESIAN_POINT('',(-3.91,-1.915,0.8));
#22372=CARTESIAN_POINT('Origin',(-0.525,-1.8893933982822,0.789393398282202));
#22373=CARTESIAN_POINT('',(-2.1,-1.915,0.8));
#22374=CARTESIAN_POINT('',(-0.525,-1.915,0.8));
#22375=CARTESIAN_POINT('',(-2.1,-1.8637867965644,0.778786796564404));
#22376=CARTESIAN_POINT('',(-2.1,-1.915,0.8));
#22377=CARTESIAN_POINT('',(-0.525,-1.8637867965644,0.778786796564404));
#22378=CARTESIAN_POINT('Origin',(-2.1,-1.5,0.789393398282202));
#22379=CARTESIAN_POINT('',(-2.1,-1.085,0.8));
#22380=CARTESIAN_POINT('',(-2.1,-1.1362132034356,0.778786796564404));
#22381=CARTESIAN_POINT('',(-2.1,-1.085,0.8));
#22382=CARTESIAN_POINT('Origin',(-2.1,-1.5,0.778786796564404));
#22383=CARTESIAN_POINT('Origin',(-2.1,-1.5,0.8));
#22384=CARTESIAN_POINT('Origin',(-1.025,-1.1106066017178,0.789393398282202));
#22385=CARTESIAN_POINT('',(-1.025,-1.1362132034356,0.778786796564404));
#22386=CARTESIAN_POINT('',(-3.91,-1.085,0.8));
#22387=CARTESIAN_POINT('',(-1.025,-1.085,0.8));
#22388=CARTESIAN_POINT('',(-3.91,-1.085,0.8));
#22389=CARTESIAN_POINT('Origin',(-3.9356066017178,0.75,0.789393398282202));
#22390=CARTESIAN_POINT('',(-3.91,1.085,0.8));
#22391=CARTESIAN_POINT('',(-3.91,0.75,0.8));
#22392=CARTESIAN_POINT('',(-3.91,1.085,0.8));
#22393=CARTESIAN_POINT('Origin',(-0.525,1.1106066017178,0.789393398282202));
#22394=CARTESIAN_POINT('',(-2.1,1.085,0.8));
#22395=CARTESIAN_POINT('',(-0.525,1.085,0.8));
#22396=CARTESIAN_POINT('',(-2.1,1.1362132034356,0.778786796564404));
#22397=CARTESIAN_POINT('',(-2.1,1.085,0.8));
#22398=CARTESIAN_POINT('',(-0.525,1.1362132034356,0.778786796564404));
#22399=CARTESIAN_POINT('Origin',(-2.1,1.5,0.789393398282202));
#22400=CARTESIAN_POINT('',(-2.1,1.915,0.8));
#22401=CARTESIAN_POINT('',(-2.1,1.915,0.8));
#22402=CARTESIAN_POINT('Origin',(-2.1,1.5,0.778786796564404));
#22403=CARTESIAN_POINT('Origin',(-2.1,1.5,0.8));
#22404=CARTESIAN_POINT('Origin',(-1.025,1.8893933982822,0.789393398282202));
#22405=CARTESIAN_POINT('',(-1.025,1.915,0.8));
#22406=CARTESIAN_POINT('Origin',(0.,0.,0.8));
#22407=CARTESIAN_POINT('',(1.75,-2.14313189850787E-16,0.8));
#22408=CARTESIAN_POINT('Origin',(0.,0.,0.8));
#22409=CARTESIAN_POINT('Ctrl Pts',(-0.2347153981354,1.58269033037993,1.4));
#22410=CARTESIAN_POINT('Ctrl Pts',(-0.2347153981354,1.58269033037993,1.36620206917426));
#22411=CARTESIAN_POINT('Ctrl Pts',(-0.217558446824302,1.5852549399837,1.29316877041114));
#22412=CARTESIAN_POINT('Ctrl Pts',(-0.152415457266674,1.59355456054094,
1.21049566567658));
#22413=CARTESIAN_POINT('Ctrl Pts',(-0.0521025187876913,1.6002700877622,
1.1629600177189));
#22414=CARTESIAN_POINT('Ctrl Pts',(0.0523288394347715,1.60033288629179,
1.1627635323513));
#22415=CARTESIAN_POINT('Ctrl Pts',(0.136901297650221,1.5944726374199,1.20393468493575));
#22416=CARTESIAN_POINT('Ctrl Pts',(0.184075177725469,1.58943902120323,1.2517856376839));
#22417=CARTESIAN_POINT('Ctrl Pts',(0.242438373304523,1.58178434531461,1.3436546039934));
#22418=CARTESIAN_POINT('Ctrl Pts',(0.242424895429431,1.58195751401911,1.45610993307891));
#22419=CARTESIAN_POINT('Ctrl Pts',(0.184096357151629,1.58953393073711,1.54838937357335));
#22420=CARTESIAN_POINT('Ctrl Pts',(0.136902935945947,1.59458452325023,1.59624390388577));
#22421=CARTESIAN_POINT('Ctrl Pts',(0.0519568849441468,1.60038159630494,
1.63731023393358));
#22422=CARTESIAN_POINT('Ctrl Pts',(-0.0517911204160937,1.60029839497895,
1.63694413004937));
#22423=CARTESIAN_POINT('Ctrl Pts',(-0.152692584771416,1.59356568559404,
1.58941995958521));
#22424=CARTESIAN_POINT('Ctrl Pts',(-0.217487941313751,1.58526334196631,
1.50680645542181));
#22425=CARTESIAN_POINT('Ctrl Pts',(-0.2347153981354,1.58269033037993,1.43379793082574));
#22426=CARTESIAN_POINT('Ctrl Pts',(-0.2347153981354,1.58269033037993,1.4));
#22427=CARTESIAN_POINT('Ctrl Pts',(-0.2248102654236,1.57406450138881,1.4));
#22428=CARTESIAN_POINT('Ctrl Pts',(-0.2248102654236,1.57406450138881,1.36746503270754));
#22429=CARTESIAN_POINT('Ctrl Pts',(-0.208168355079963,1.57643917618978,
1.29717176826053));
#22430=CARTESIAN_POINT('Ctrl Pts',(-0.145352583133322,1.58409368553478,
1.21811904501364));
#22431=CARTESIAN_POINT('Ctrl Pts',(-0.0495346081425047,1.59024754799312,
1.17306430934237));
#22432=CARTESIAN_POINT('Ctrl Pts',(0.0497577306442636,1.5903054545027,1.17287877730999));
#22433=CARTESIAN_POINT('Ctrl Pts',(0.13056132404074,1.58493199888725,1.21191562354324));
#22434=CARTESIAN_POINT('Ctrl Pts',(0.175895886034792,1.58029752812982,1.25760296158226));
#22435=CARTESIAN_POINT('Ctrl Pts',(0.232247513828916,1.573229487498,1.34562917220083));
#22436=CARTESIAN_POINT('Ctrl Pts',(0.232200074131124,1.57339191262612,1.45414529678908));
#22437=CARTESIAN_POINT('Ctrl Pts',(0.17589638642471,1.58038666110775,1.54256638101033));
#22438=CARTESIAN_POINT('Ctrl Pts',(0.130540644251271,1.58503685490416,1.58825637023856));
#22439=CARTESIAN_POINT('Ctrl Pts',(0.049394174333855,1.5903513019701,1.62719353838594));
#22440=CARTESIAN_POINT('Ctrl Pts',(-0.049245443635495,1.59027401139424,
1.62684329859291));
#22441=CARTESIAN_POINT('Ctrl Pts',(-0.145615679686565,1.58410410610257,
1.5817991026622));
#22442=CARTESIAN_POINT('Ctrl Pts',(-0.208103245541503,1.57644703442885,
1.50280434314757));
#22443=CARTESIAN_POINT('Ctrl Pts',(-0.2248102654236,1.57406450138881,1.43253496729245));
#22444=CARTESIAN_POINT('Ctrl Pts',(-0.2248102654236,1.57406450138881,1.4));
#22445=CARTESIAN_POINT('Ctrl Pts',(-0.2149051327118,1.56543867239768,1.4));
#22446=CARTESIAN_POINT('Ctrl Pts',(-0.2149051327118,1.56543867239768,1.36872799624083));
#22447=CARTESIAN_POINT('Ctrl Pts',(-0.198778263335623,1.56762341239587,
1.30117476610993));
#22448=CARTESIAN_POINT('Ctrl Pts',(-0.138289708999972,1.57463281052862,
1.22574242435069));
#22449=CARTESIAN_POINT('Ctrl Pts',(-0.0469666974973182,1.58022500822404,
1.18316860096584));
#22450=CARTESIAN_POINT('Ctrl Pts',(0.0471866218537556,1.58027802271362,
1.18299402226868));
#22451=CARTESIAN_POINT('Ctrl Pts',(0.12422135043126,1.5753913603546,1.21989656215073));
#22452=CARTESIAN_POINT('Ctrl Pts',(0.167716594344116,1.57115603505641,1.26342028548062));
#22453=CARTESIAN_POINT('Ctrl Pts',(0.222056654353309,1.5646746296814,1.34760374040825));
#22454=CARTESIAN_POINT('Ctrl Pts',(0.221975252832816,1.56482631123312,1.45218066049925));
#22455=CARTESIAN_POINT('Ctrl Pts',(0.167696415697792,1.5712393914784,1.53674338844731));
#22456=CARTESIAN_POINT('Ctrl Pts',(0.124178352556595,1.5754891865581,1.58026883659135));
#22457=CARTESIAN_POINT('Ctrl Pts',(0.0468314637235632,1.58032100763526,
1.61707684283829));
#22458=CARTESIAN_POINT('Ctrl Pts',(-0.0466997668548959,1.58024962780953,
1.61674246713645));
#22459=CARTESIAN_POINT('Ctrl Pts',(-0.138538774601714,1.57464252661111,
1.57417824573919));
#22460=CARTESIAN_POINT('Ctrl Pts',(-0.198718549769256,1.56763072689139,
1.49880223087334));
#22461=CARTESIAN_POINT('Ctrl Pts',(-0.2149051327118,1.56543867239768,1.43127200375917));
#22462=CARTESIAN_POINT('Ctrl Pts',(-0.2149051327118,1.56543867239768,1.4));
#22463=CARTESIAN_POINT('Ctrl Pts',(-0.205,1.55681284340656,1.4));
#22464=CARTESIAN_POINT('Ctrl Pts',(-0.205,1.55681284340656,1.36999095977411));
#22465=CARTESIAN_POINT('Ctrl Pts',(-0.189388171591284,1.55880764860196,
1.30517776395932));
#22466=CARTESIAN_POINT('Ctrl Pts',(-0.131226834866621,1.56517193552246,
1.23336580368775));
#22467=CARTESIAN_POINT('Ctrl Pts',(-0.0443987868521316,1.57020246845496,
1.19327289258931));
#22468=CARTESIAN_POINT('Ctrl Pts',(0.0446155130632477,1.57025059092453,
1.19310926722737));
#22469=CARTESIAN_POINT('Ctrl Pts',(0.11788137682178,1.56585072182196,1.22787750075822));
#22470=CARTESIAN_POINT('Ctrl Pts',(0.15953730265344,1.56201454198299,1.26923760937899));
#22471=CARTESIAN_POINT('Ctrl Pts',(0.211865794877702,1.55611977186479,1.34957830861567));
#22472=CARTESIAN_POINT('Ctrl Pts',(0.211750431534509,1.55626070984013,1.45021602420942));
#22473=CARTESIAN_POINT('Ctrl Pts',(0.159496444970874,1.56209212184905,1.53092039588429));
#22474=CARTESIAN_POINT('Ctrl Pts',(0.117816060861919,1.56594151821204,1.57228130294414));
#22475=CARTESIAN_POINT('Ctrl Pts',(0.0442687531132715,1.57029071330042,
1.60696014729065));
#22476=CARTESIAN_POINT('Ctrl Pts',(-0.0441540900742972,1.57022524422482,
1.60664163567999));
#22477=CARTESIAN_POINT('Ctrl Pts',(-0.131461869516863,1.56518094711964,
1.56655738881618));
#22478=CARTESIAN_POINT('Ctrl Pts',(-0.189333853997008,1.55881441935392,
1.49480011859911));
#22479=CARTESIAN_POINT('Ctrl Pts',(-0.205,1.55681284340656,1.43000904022589));
#22480=CARTESIAN_POINT('Ctrl Pts',(-0.205,1.55681284340656,1.4));
#22481=CARTESIAN_POINT('',(-0.2347153981354,1.58269033037993,1.4));
#22482=CARTESIAN_POINT('',(-0.2347153981354,1.58269033037993,1.4));
#22483=CARTESIAN_POINT('Ctrl Pts',(-0.2347153981354,1.58269033037993,1.4));
#22484=CARTESIAN_POINT('Ctrl Pts',(-0.2347153981354,1.58269033037993,1.43379793082574));
#22485=CARTESIAN_POINT('Ctrl Pts',(-0.217487941313751,1.58526334196631,
1.50680645542181));
#22486=CARTESIAN_POINT('Ctrl Pts',(-0.152692584771416,1.59356568559404,
1.58941995958521));
#22487=CARTESIAN_POINT('Ctrl Pts',(-0.0517911204160937,1.60029839497895,
1.63694413004937));
#22488=CARTESIAN_POINT('Ctrl Pts',(0.0519568849441468,1.60038159630494,
1.63731023393358));
#22489=CARTESIAN_POINT('Ctrl Pts',(0.136902935945947,1.59458452325023,1.59624390388577));
#22490=CARTESIAN_POINT('Ctrl Pts',(0.184096357151629,1.58953393073711,1.54838937357335));
#22491=CARTESIAN_POINT('Ctrl Pts',(0.242424895429431,1.58195751401911,1.45610993307891));
#22492=CARTESIAN_POINT('Ctrl Pts',(0.242438373304523,1.58178434531461,1.3436546039934));
#22493=CARTESIAN_POINT('Ctrl Pts',(0.184075177725469,1.58943902120323,1.2517856376839));
#22494=CARTESIAN_POINT('Ctrl Pts',(0.136901297650221,1.5944726374199,1.20393468493575));
#22495=CARTESIAN_POINT('Ctrl Pts',(0.0523288394347715,1.60033288629179,
1.1627635323513));
#22496=CARTESIAN_POINT('Ctrl Pts',(-0.0521025187876913,1.6002700877622,
1.1629600177189));
#22497=CARTESIAN_POINT('Ctrl Pts',(-0.152415457266674,1.59355456054094,
1.21049566567658));
#22498=CARTESIAN_POINT('Ctrl Pts',(-0.217558446824302,1.5852549399837,1.29316877041114));
#22499=CARTESIAN_POINT('Ctrl Pts',(-0.2347153981354,1.58269033037993,1.36620206917426));
#22500=CARTESIAN_POINT('Ctrl Pts',(-0.2347153981354,1.58269033037993,1.4));
#22501=CARTESIAN_POINT('Origin',(0.,0.,0.8));
#22502=CARTESIAN_POINT('',(-1.6,-1.95943487863577E-16,1.91));
#22503=CARTESIAN_POINT('Origin',(0.,0.,1.91));
#22504=CARTESIAN_POINT('',(-1.6,1.95943487863577E-16,0.95));
#22505=CARTESIAN_POINT('',(-1.6,-1.95943487863577E-16,0.8));
#22506=CARTESIAN_POINT('',(1.6,-1.95943487863577E-16,0.95));
#22507=CARTESIAN_POINT('Origin',(0.,0.,0.95));
#22508=CARTESIAN_POINT('Origin',(0.,0.,0.95));
#22509=CARTESIAN_POINT('Origin',(0.,-4.83364049237175E-17,1.9356066017178));
#22510=CARTESIAN_POINT('',(-1.5787867965644,0.,1.9612132034356));
#22511=CARTESIAN_POINT('Origin',(0.,-9.6672809847435E-17,1.9612132034356));
#22512=CARTESIAN_POINT('',(-1.5893933982822,-2.91317363626658E-16,1.9356066017178));
#22513=CARTESIAN_POINT('Origin',(0.,0.,1.97));
#22514=CARTESIAN_POINT('',(-1.57,-1.92269547466134E-16,1.97));
#22515=CARTESIAN_POINT('Origin',(0.,0.,0.95));
#22516=CARTESIAN_POINT('Origin',(1.75,-2.14313189850787E-16,0.95));
#22517=CARTESIAN_POINT('Origin',(0.,0.,0.4));
#22518=CARTESIAN_POINT('Origin',(3.98,-1.5,0.02));
#22519=CARTESIAN_POINT('',(3.96,1.865,0.));
#22520=CARTESIAN_POINT('',(4.,1.825,0.04));
#22521=CARTESIAN_POINT('',(3.96,2.6,0.));
#22522=CARTESIAN_POINT('',(3.96,-1.5,0.));
#22523=CARTESIAN_POINT('',(3.96,2.6,0.));
#22524=CARTESIAN_POINT('Origin',(3.98,-1.5,0.02));
#22525=CARTESIAN_POINT('',(3.96,-1.135,0.));
#22526=CARTESIAN_POINT('',(4.,-1.175,0.04));
#22527=CARTESIAN_POINT('',(3.96,1.135,0.));
#22528=CARTESIAN_POINT('',(3.96,-1.5,0.));
#22529=CARTESIAN_POINT('',(3.96,1.135,0.));
#22530=CARTESIAN_POINT('Origin',(-3.6,-2.6,0.02));
#22531=CARTESIAN_POINT('',(-3.6,-2.96,0.));
#22532=CARTESIAN_POINT('',(-3.6,-3.,0.04));
#22533=CARTESIAN_POINT('',(-3.6,-2.96,0.));
#22534=CARTESIAN_POINT('Origin',(-3.6,-2.6,0.04));
#22535=CARTESIAN_POINT('Origin',(-3.6,-2.6,0.));
#22536=CARTESIAN_POINT('Origin',(-2.,-2.98,0.02));
#22537=CARTESIAN_POINT('',(3.6,-2.96,0.));
#22538=CARTESIAN_POINT('',(3.6,-3.,0.04));
#22539=CARTESIAN_POINT('',(3.6,-2.96,0.));
#22540=CARTESIAN_POINT('',(-2.,-3.,0.04));
#22541=CARTESIAN_POINT('',(-2.,-2.96,0.));
#22542=CARTESIAN_POINT('Origin',(3.6,-2.6,0.02));
#22543=CARTESIAN_POINT('',(3.96,-2.6,0.));
#22544=CARTESIAN_POINT('',(3.96,-2.6,0.));
#22545=CARTESIAN_POINT('Origin',(3.6,-2.6,0.04));
#22546=CARTESIAN_POINT('Origin',(3.6,-2.6,0.));
#22547=CARTESIAN_POINT('Origin',(3.98,-1.5,0.02));
#22548=CARTESIAN_POINT('',(3.96,-1.865,0.));
#22549=CARTESIAN_POINT('',(3.96,-1.5,0.));
#22550=CARTESIAN_POINT('',(3.96,-1.865,0.));
#22551=CARTESIAN_POINT('Origin',(-1.05,-1.845,0.02));
#22552=CARTESIAN_POINT('',(-2.1,-1.825,0.04));
#22553=CARTESIAN_POINT('',(-1.05,-1.825,0.04));
#22554=CARTESIAN_POINT('',(-2.1,-1.865,0.));
#22555=CARTESIAN_POINT('',(-2.1,-1.825,0.04));
#22556=CARTESIAN_POINT('',(-1.05,-1.865,0.));
#22557=CARTESIAN_POINT('Origin',(-2.1,-1.5,0.02));
#22558=CARTESIAN_POINT('',(-2.1,-1.175,0.04));
#22559=CARTESIAN_POINT('',(-2.1,-1.135,0.));
#22560=CARTESIAN_POINT('',(-2.1,-1.175,0.04));
#22561=CARTESIAN_POINT('Origin',(-2.1,-1.5,0.));
#22562=CARTESIAN_POINT('Origin',(-2.1,-1.5,0.04));
#22563=CARTESIAN_POINT('Origin',(-2.05,-1.155,0.02));
#22564=CARTESIAN_POINT('',(-2.05,-1.135,0.));
#22565=CARTESIAN_POINT('',(-2.05,-1.175,0.04));
#22566=CARTESIAN_POINT('Origin',(1.05,-1.155,0.02));
#22567=CARTESIAN_POINT('',(2.1,-1.175,0.04));
#22568=CARTESIAN_POINT('',(1.05,-1.175,0.04));
#22569=CARTESIAN_POINT('',(2.1,-1.135,0.));
#22570=CARTESIAN_POINT('',(2.1,-1.175,0.04));
#22571=CARTESIAN_POINT('',(1.05,-1.135,0.));
#22572=CARTESIAN_POINT('Origin',(2.1,-1.5,0.02));
#22573=CARTESIAN_POINT('',(2.1,-1.825,0.04));
#22574=CARTESIAN_POINT('',(2.1,-1.865,0.));
#22575=CARTESIAN_POINT('',(2.1,-1.825,0.04));
#22576=CARTESIAN_POINT('Origin',(2.1,-1.5,0.));
#22577=CARTESIAN_POINT('Origin',(2.1,-1.5,0.04));
#22578=CARTESIAN_POINT('Origin',(2.05,-1.845,0.02));
#22579=CARTESIAN_POINT('',(2.05,-1.865,0.));
#22580=CARTESIAN_POINT('',(2.05,-1.825,0.04));
#22581=CARTESIAN_POINT('Origin',(-1.05,1.155,0.02));
#22582=CARTESIAN_POINT('',(-2.1,1.175,0.04));
#22583=CARTESIAN_POINT('',(-1.05,1.175,0.04));
#22584=CARTESIAN_POINT('',(-2.1,1.135,0.));
#22585=CARTESIAN_POINT('',(-2.1,1.175,0.04));
#22586=CARTESIAN_POINT('',(-1.05,1.135,0.));
#22587=CARTESIAN_POINT('Origin',(-2.1,1.5,0.02));
#22588=CARTESIAN_POINT('',(-2.1,1.865,0.));
#22589=CARTESIAN_POINT('',(-2.1,1.825,0.04));
#22590=CARTESIAN_POINT('Origin',(-2.1,1.5,0.));
#22591=CARTESIAN_POINT('Origin',(-2.1,1.5,0.04));
#22592=CARTESIAN_POINT('Origin',(-2.05,1.845,0.02));
#22593=CARTESIAN_POINT('',(-2.05,1.865,0.));
#22594=CARTESIAN_POINT('Origin',(1.05,1.845,0.02));
#22595=CARTESIAN_POINT('',(2.1,1.865,0.));
#22596=CARTESIAN_POINT('',(2.1,1.825,0.04));
#22597=CARTESIAN_POINT('',(1.05,1.865,0.));
#22598=CARTESIAN_POINT('Origin',(2.1,1.5,0.02));
#22599=CARTESIAN_POINT('',(2.1,1.175,0.04));
#22600=CARTESIAN_POINT('',(2.1,1.135,0.));
#22601=CARTESIAN_POINT('',(2.1,1.175,0.04));
#22602=CARTESIAN_POINT('Origin',(2.1,1.5,0.));
#22603=CARTESIAN_POINT('Origin',(2.1,1.5,0.04));
#22604=CARTESIAN_POINT('Origin',(2.05,1.155,0.02));
#22605=CARTESIAN_POINT('',(2.05,1.135,0.));
#22606=CARTESIAN_POINT('',(2.05,1.175,0.04));
#22607=CARTESIAN_POINT('Origin',(3.6,2.6,0.02));
#22608=CARTESIAN_POINT('',(3.6,2.96,0.));
#22609=CARTESIAN_POINT('',(3.6,2.96,0.));
#22610=CARTESIAN_POINT('Origin',(3.6,2.6,0.));
#22611=CARTESIAN_POINT('Origin',(2.,2.98,0.02));
#22612=CARTESIAN_POINT('',(-3.6,2.96,0.));
#22613=CARTESIAN_POINT('',(-3.6,2.96,0.));
#22614=CARTESIAN_POINT('',(2.,2.96,0.));
#22615=CARTESIAN_POINT('Origin',(-3.6,2.6,0.02));
#22616=CARTESIAN_POINT('Origin',(-3.6,2.6,0.));
#22617=CARTESIAN_POINT('Origin',(-2.1,1.5,0.8));
#22618=CARTESIAN_POINT('',(-2.1,1.175,0.74));
#22619=CARTESIAN_POINT('',(-2.1,1.175,0.8));
#22620=CARTESIAN_POINT('Origin',(-2.1,1.5,0.74));
#22621=CARTESIAN_POINT('Origin',(-2.1,1.175,0.8));
#22622=CARTESIAN_POINT('',(-1.05,1.175,0.74));
#22623=CARTESIAN_POINT('Origin',(-4.1,-1.175,0.8));
#22624=CARTESIAN_POINT('',(-2.1,-1.175,0.74));
#22625=CARTESIAN_POINT('',(-2.1,-1.175,0.8));
#22626=CARTESIAN_POINT('',(-2.05,-1.175,0.74));
#22627=CARTESIAN_POINT('Origin',(-2.1,-1.5,0.8));
#22628=CARTESIAN_POINT('',(-2.1,-1.825,0.74));
#22629=CARTESIAN_POINT('',(-2.1,-1.825,0.8));
#22630=CARTESIAN_POINT('Origin',(-2.1,-1.5,0.74));
#22631=CARTESIAN_POINT('Origin',(-2.1,-1.825,0.8));
#22632=CARTESIAN_POINT('',(-1.05,-1.825,0.74));
#22633=CARTESIAN_POINT('Origin',(0.,0.,0.));
#22634=CARTESIAN_POINT('Origin',(-3.6,-2.6,0.77));
#22635=CARTESIAN_POINT('',(-3.6,-3.,0.74));
#22636=CARTESIAN_POINT('Origin',(-3.6,-2.6,0.74));
#22637=CARTESIAN_POINT('',(-3.6,-3.,0.74));
#22638=CARTESIAN_POINT('Origin',(-2.,-2.97,0.77));
#22639=CARTESIAN_POINT('',(3.6,-3.,0.74));
#22640=CARTESIAN_POINT('',(-2.,-3.,0.74));
#22641=CARTESIAN_POINT('',(3.6,-3.,0.74));
#22642=CARTESIAN_POINT('Origin',(3.6,-2.6,0.77));
#22643=CARTESIAN_POINT('Origin',(3.6,-2.6,0.74));
#22644=CARTESIAN_POINT('Origin',(-2.05,-1.145,0.77));
#22645=CARTESIAN_POINT('',(-2.1,-1.175,0.74));
#22646=CARTESIAN_POINT('Origin',(-2.1,-1.5,0.77));
#22647=CARTESIAN_POINT('',(-2.1,-1.825,0.74));
#22648=CARTESIAN_POINT('Origin',(-1.05,-1.855,0.77));
#22649=CARTESIAN_POINT('Origin',(2.1,-1.5,0.77));
#22650=CARTESIAN_POINT('Origin',(2.1,-1.5,0.74));
#22651=CARTESIAN_POINT('Origin',(-2.1,1.5,0.77));
#22652=CARTESIAN_POINT('',(-2.1,1.175,0.74));
#22653=CARTESIAN_POINT('Origin',(-1.05,1.145,0.77));
#22654=CARTESIAN_POINT('Origin',(2.1,1.5,0.77));
#22655=CARTESIAN_POINT('Origin',(2.1,1.5,0.74));
#22656=CARTESIAN_POINT('Origin',(3.6,-2.6,0.));
#22657=CARTESIAN_POINT('',(3.6,-3.,0.));
#22658=CARTESIAN_POINT('Origin',(-4.,-3.,0.));
#22659=CARTESIAN_POINT('',(-3.6,-3.,0.));
#22660=CARTESIAN_POINT('Origin',(-3.6,-2.6,0.));
#22661=CARTESIAN_POINT('Origin',(4.1,1.175,0.8));
#22662=CARTESIAN_POINT('',(2.1,1.175,0.8));
#22663=CARTESIAN_POINT('Origin',(2.1,1.5,0.8));
#22664=CARTESIAN_POINT('Origin',(4.1,-1.825,0.8));
#22665=CARTESIAN_POINT('',(2.1,-1.825,0.8));
#22666=CARTESIAN_POINT('Origin',(2.1,-1.175,0.8));
#22667=CARTESIAN_POINT('',(2.1,-1.175,0.8));
#22668=CARTESIAN_POINT('Origin',(2.1,-1.5,0.8));
#22669=CARTESIAN_POINT('',(0.,0.,0.));
#22670=CARTESIAN_POINT('Origin',(-1.2,0.,3.4));
#22671=CARTESIAN_POINT('',(-1.2,-5.32721357629099E-17,2.965));
#22672=CARTESIAN_POINT('Origin',(-1.2,0.,3.4));
#22673=CARTESIAN_POINT('',(-1.2,2.51052593825207E-17,3.195));
#22674=CARTESIAN_POINT('Origin',(-1.2,0.,3.4));
#22675=CARTESIAN_POINT('Origin',(-0.9825,0.,3.4));
#22676=CARTESIAN_POINT('',(-0.97,-2.51052593825207E-17,3.195));
#22677=CARTESIAN_POINT('Origin',(-0.97,0.,3.4));
#22678=CARTESIAN_POINT('',(-0.9825,-2.66360678814549E-17,3.1825));
#22679=CARTESIAN_POINT('Origin',(-1.0025,0.,3.4));
#22680=CARTESIAN_POINT('',(-0.675,-0.203469899493758,3.425));
#22681=CARTESIAN_POINT('',(-0.705,-4.31687996699442E-17,3.605));
#22682=CARTESIAN_POINT('Ctrl Pts',(-0.675,-0.203469899493758,3.425));
#22683=CARTESIAN_POINT('Ctrl Pts',(-0.675671543655374,-0.201242091014444,
3.44313167869509));
#22684=CARTESIAN_POINT('Ctrl Pts',(-0.677111481787171,-0.196469587434997,
3.46142442095761));
#22685=CARTESIAN_POINT('Ctrl Pts',(-0.682029730751166,-0.178826374035794,
3.50388715643587));
#22686=CARTESIAN_POINT('Ctrl Pts',(-0.68612968485916,-0.16307623613103,
3.52683754415545));
#22687=CARTESIAN_POINT('Ctrl Pts',(-0.693742502155627,-0.126842282640148,
3.56307149764634));
#22688=CARTESIAN_POINT('Ctrl Pts',(-0.697765433634744,-0.103889959828094,
3.57882531009039));
#22689=CARTESIAN_POINT('Ctrl Pts',(-0.703431290629093,-0.0534241842031802,
3.59979357492158));
#22690=CARTESIAN_POINT('Ctrl Pts',(-0.705,-0.0258990920208441,3.605));
#22691=CARTESIAN_POINT('Ctrl Pts',(-0.705,-2.42861286636753E-17,3.605));
#22692=CARTESIAN_POINT('',(-0.675,-0.203469899493758,3.375));
#22693=CARTESIAN_POINT('Origin',(-0.675,0.,3.4));
#22694=CARTESIAN_POINT('',(-0.705,4.79460506850772E-18,3.195));
#22695=CARTESIAN_POINT('Ctrl Pts',(-0.705,3.46944695195361E-17,3.195));
#22696=CARTESIAN_POINT('Ctrl Pts',(-0.705,-0.0258990920208441,3.195));
#22697=CARTESIAN_POINT('Ctrl Pts',(-0.703431290629093,-0.0534241842031802,
3.20020642507842));
#22698=CARTESIAN_POINT('Ctrl Pts',(-0.697765433634744,-0.103889959828094,
3.22117468990961));
#22699=CARTESIAN_POINT('Ctrl Pts',(-0.693742502155627,-0.126842282640148,
3.23692850235366));
#22700=CARTESIAN_POINT('Ctrl Pts',(-0.68612968485916,-0.16307623613103,
3.27316245584455));
#22701=CARTESIAN_POINT('Ctrl Pts',(-0.682029730751167,-0.178826374035794,
3.29611284356413));
#22702=CARTESIAN_POINT('Ctrl Pts',(-0.677111481787171,-0.196469587434997,
3.33857557904239));
#22703=CARTESIAN_POINT('Ctrl Pts',(-0.675671543655374,-0.201242091014444,
3.35686832130491));
#22704=CARTESIAN_POINT('Ctrl Pts',(-0.675,-0.203469899493758,3.375));
#22705=CARTESIAN_POINT('',(-1.0025,-2.51052593825207E-17,3.195));
#22706=CARTESIAN_POINT('',(-0.675,0.203469899493758,3.375));
#22707=CARTESIAN_POINT('Ctrl Pts',(-0.675,0.203469899493758,3.375));
#22708=CARTESIAN_POINT('Ctrl Pts',(-0.675671543655374,0.201242091014444,
3.35686832130491));
#22709=CARTESIAN_POINT('Ctrl Pts',(-0.677111481787171,0.196469587434997,
3.33857557904239));
#22710=CARTESIAN_POINT('Ctrl Pts',(-0.682029730751166,0.178826374035794,
3.29611284356413));
#22711=CARTESIAN_POINT('Ctrl Pts',(-0.68612968485916,0.16307623613103,3.27316245584455));
#22712=CARTESIAN_POINT('Ctrl Pts',(-0.693742502155627,0.126842282640148,
3.23692850235366));
#22713=CARTESIAN_POINT('Ctrl Pts',(-0.697765433634744,0.103889959828094,
3.22117468990961));
#22714=CARTESIAN_POINT('Ctrl Pts',(-0.703431290629093,0.0534241842031802,
3.20020642507842));
#22715=CARTESIAN_POINT('Ctrl Pts',(-0.705,0.025899092020844,3.195));
#22716=CARTESIAN_POINT('Ctrl Pts',(-0.705,-4.16333634234434E-17,3.195));
#22717=CARTESIAN_POINT('',(-0.675,0.203469899493758,3.425));
#22718=CARTESIAN_POINT('Origin',(-0.675,0.,3.4));
#22719=CARTESIAN_POINT('Ctrl Pts',(-0.705,0.,3.605));
#22720=CARTESIAN_POINT('Ctrl Pts',(-0.705,0.025899092020844,3.605));
#22721=CARTESIAN_POINT('Ctrl Pts',(-0.703431290629093,0.0534241842031802,
3.59979357492158));
#22722=CARTESIAN_POINT('Ctrl Pts',(-0.697765433634744,0.103889959828094,
3.57882531009039));
#22723=CARTESIAN_POINT('Ctrl Pts',(-0.693742502155627,0.126842282640148,
3.56307149764634));
#22724=CARTESIAN_POINT('Ctrl Pts',(-0.68612968485916,0.16307623613103,3.52683754415545));
#22725=CARTESIAN_POINT('Ctrl Pts',(-0.682029730751166,0.178826374035794,
3.50388715643587));
#22726=CARTESIAN_POINT('Ctrl Pts',(-0.67711148178717,0.196469587434997,
3.46142442095761));
#22727=CARTESIAN_POINT('Ctrl Pts',(-0.675671543655374,0.201242091014444,
3.44313167869509));
#22728=CARTESIAN_POINT('Ctrl Pts',(-0.675,0.203469899493758,3.425));
#22729=CARTESIAN_POINT('Origin',(0.,-1.2,3.4));
#22730=CARTESIAN_POINT('',(-5.32721357629099E-17,-1.2,2.965));
#22731=CARTESIAN_POINT('Origin',(0.,-1.2,3.4));
#22732=CARTESIAN_POINT('',(2.51052593825207E-17,-0.97,3.195));
#22733=CARTESIAN_POINT('',(-5.32721357629099E-17,-1.2,2.965));
#22734=CARTESIAN_POINT('Origin',(0.,-0.97,3.4));
#22735=CARTESIAN_POINT('Origin',(0.,-1.2,3.835));
#22736=CARTESIAN_POINT('',(-2.51052593825207E-17,-1.2,3.195));
#22737=CARTESIAN_POINT('Origin',(0.,-1.2,3.4));
#22738=CARTESIAN_POINT('Origin',(0.,-1.0025,3.4));
#22739=CARTESIAN_POINT('',(-0.205,-1.28373478569368,3.4));
#22740=CARTESIAN_POINT('',(-2.51052593825207E-17,-1.3,3.195));
#22741=CARTESIAN_POINT('Ctrl Pts',(-0.205,-1.28373478569368,3.4));
#22742=CARTESIAN_POINT('Ctrl Pts',(-0.205,-1.28373478569368,3.42578682852176));
#22743=CARTESIAN_POINT('Ctrl Pts',(-0.199837668299145,-1.28459209201807,
3.45326250834418));
#22744=CARTESIAN_POINT('Ctrl Pts',(-0.178903418830812,-1.2876744550022,
3.50375720035387));
#22745=CARTESIAN_POINT('Ctrl Pts',(-0.163133809500307,-1.28985344916615,
3.52677997078618));
#22746=CARTESIAN_POINT('Ctrl Pts',(-0.12678035877662,-1.29393248914849,
3.56313342150986));
#22747=CARTESIAN_POINT('Ctrl Pts',(-0.103757421316811,-1.29609960028466,
3.57890333519745));
#22748=CARTESIAN_POINT('Ctrl Pts',(-0.0532621572488602,-1.29915469398922,
3.59983780588318));
#22749=CARTESIAN_POINT('Ctrl Pts',(-0.0257862780960919,-1.3,3.605));
#22750=CARTESIAN_POINT('Ctrl Pts',(0.0257862780960919,-1.3,3.605));
#22751=CARTESIAN_POINT('Ctrl Pts',(0.0532621572488602,-1.29915469398922,
3.59983780588318));
#22752=CARTESIAN_POINT('Ctrl Pts',(0.103757421316811,-1.29609960028466,
3.57890333519745));
#22753=CARTESIAN_POINT('Ctrl Pts',(0.12678035877662,-1.29393248914849,3.56313342150986));
#22754=CARTESIAN_POINT('Ctrl Pts',(0.163133809500307,-1.28985344916615,
3.52677997078618));
#22755=CARTESIAN_POINT('Ctrl Pts',(0.178903418830811,-1.2876744550022,3.50375720035387));
#22756=CARTESIAN_POINT('Ctrl Pts',(0.199837668299145,-1.28459209201807,
3.45326250834418));
#22757=CARTESIAN_POINT('Ctrl Pts',(0.205,-1.28373478569368,3.42578682852176));
#22758=CARTESIAN_POINT('Ctrl Pts',(0.205,-1.28373478569368,3.37421317147824));
#22759=CARTESIAN_POINT('Ctrl Pts',(0.199837668299145,-1.28459209201807,
3.34673749165582));
#22760=CARTESIAN_POINT('Ctrl Pts',(0.178903418830812,-1.2876744550022,3.29624279964613));
#22761=CARTESIAN_POINT('Ctrl Pts',(0.163133809500307,-1.28985344916615,
3.27322002921382));
#22762=CARTESIAN_POINT('Ctrl Pts',(0.12678035877662,-1.29393248914849,3.23686657849014));
#22763=CARTESIAN_POINT('Ctrl Pts',(0.103757421316811,-1.29609960028466,
3.22109666480255));
#22764=CARTESIAN_POINT('Ctrl Pts',(0.0532621572488603,-1.29915469398922,
3.20016219411682));
#22765=CARTESIAN_POINT('Ctrl Pts',(0.025786278096092,-1.3,3.195));
#22766=CARTESIAN_POINT('Ctrl Pts',(5.55111512312578E-17,-1.3,3.195));
#22767=CARTESIAN_POINT('Ctrl Pts',(3.81639164714898E-17,-1.3,3.195));
#22768=CARTESIAN_POINT('Ctrl Pts',(-0.0257862780960919,-1.3,3.195));
#22769=CARTESIAN_POINT('Ctrl Pts',(-0.0532621572488602,-1.29915469398922,
3.20016219411682));
#22770=CARTESIAN_POINT('Ctrl Pts',(-0.103757421316811,-1.29609960028466,
3.22109666480255));
#22771=CARTESIAN_POINT('Ctrl Pts',(-0.12678035877662,-1.29393248914849,
3.23686657849014));
#22772=CARTESIAN_POINT('Ctrl Pts',(-0.163133809500307,-1.28985344916615,
3.27322002921382));
#22773=CARTESIAN_POINT('Ctrl Pts',(-0.178903418830812,-1.2876744550022,
3.29624279964613));
#22774=CARTESIAN_POINT('Ctrl Pts',(-0.199837668299145,-1.28459209201807,
3.34673749165582));
#22775=CARTESIAN_POINT('Ctrl Pts',(-0.205,-1.28373478569368,3.37421317147824));
#22776=CARTESIAN_POINT('Ctrl Pts',(-0.205,-1.28373478569368,3.4));
#22777=CARTESIAN_POINT('',(-2.51052593825207E-17,-1.0025,3.195));
#22778=CARTESIAN_POINT('Origin',(-0.675,0.,3.605));
#22779=CARTESIAN_POINT('',(-0.675,-0.203469899493758,2.275));
#22780=CARTESIAN_POINT('Origin',(-0.675,0.,3.605));
#22781=CARTESIAN_POINT('',(-0.675,0.203469899493758,2.275));
#22782=CARTESIAN_POINT('Origin',(-1.0025,0.,3.4));
#22783=CARTESIAN_POINT('',(-1.3,-2.51052593825207E-17,3.195));
#22784=CARTESIAN_POINT('',(-1.0025,-2.51052593825207E-17,3.195));
#22785=CARTESIAN_POINT('',(-1.28373478569368,-0.205,3.4));
#22786=CARTESIAN_POINT('Ctrl Pts',(-1.28373478569368,-0.205,3.4));
#22787=CARTESIAN_POINT('Ctrl Pts',(-1.28373478569368,-0.205,3.37421317147824));
#22788=CARTESIAN_POINT('Ctrl Pts',(-1.28459209201807,-0.199837668299145,
3.34673749165582));
#22789=CARTESIAN_POINT('Ctrl Pts',(-1.2876744550022,-0.178903418830812,
3.29624279964613));
#22790=CARTESIAN_POINT('Ctrl Pts',(-1.28985344916615,-0.163133809500307,
3.27322002921382));
#22791=CARTESIAN_POINT('Ctrl Pts',(-1.29393248914849,-0.12678035877662,
3.23686657849014));
#22792=CARTESIAN_POINT('Ctrl Pts',(-1.29609960028466,-0.103757421316811,
3.22109666480255));
#22793=CARTESIAN_POINT('Ctrl Pts',(-1.29915469398922,-0.0532621572488602,
3.20016219411682));
#22794=CARTESIAN_POINT('Ctrl Pts',(-1.3,-0.0257862780960919,3.195));
#22795=CARTESIAN_POINT('Ctrl Pts',(-1.3,-1.73472347597681E-17,3.195));
#22796=CARTESIAN_POINT('',(-1.3,-5.18464663289491E-17,3.605));
#22797=CARTESIAN_POINT('Ctrl Pts',(-1.3,5.55111512312578E-17,3.605));
#22798=CARTESIAN_POINT('Ctrl Pts',(-1.3,-0.0257862780960919,3.605));
#22799=CARTESIAN_POINT('Ctrl Pts',(-1.29915469398922,-0.0532621572488602,
3.59983780588318));
#22800=CARTESIAN_POINT('Ctrl Pts',(-1.29609960028466,-0.103757421316811,
3.57890333519745));
#22801=CARTESIAN_POINT('Ctrl Pts',(-1.29393248914849,-0.12678035877662,
3.56313342150986));
#22802=CARTESIAN_POINT('Ctrl Pts',(-1.28985344916615,-0.163133809500307,
3.52677997078618));
#22803=CARTESIAN_POINT('Ctrl Pts',(-1.2876744550022,-0.178903418830812,
3.50375720035387));
#22804=CARTESIAN_POINT('Ctrl Pts',(-1.28459209201807,-0.199837668299145,
3.45326250834418));
#22805=CARTESIAN_POINT('Ctrl Pts',(-1.28373478569368,-0.205,3.42578682852176));
#22806=CARTESIAN_POINT('Ctrl Pts',(-1.28373478569368,-0.205,3.4));
#22807=CARTESIAN_POINT('Ctrl Pts',(-1.3,-2.77555756156289E-17,3.195));
#22808=CARTESIAN_POINT('Ctrl Pts',(-1.3,0.0257862780960919,3.195));
#22809=CARTESIAN_POINT('Ctrl Pts',(-1.29915469398922,0.0532621572488602,
3.20016219411682));
#22810=CARTESIAN_POINT('Ctrl Pts',(-1.29609960028466,0.103757421316811,
3.22109666480255));
#22811=CARTESIAN_POINT('Ctrl Pts',(-1.29393248914849,0.12678035877662,3.23686657849014));
#22812=CARTESIAN_POINT('Ctrl Pts',(-1.28985344916615,0.163133809500307,
3.27322002921382));
#22813=CARTESIAN_POINT('Ctrl Pts',(-1.2876744550022,0.178903418830812,3.29624279964613));
#22814=CARTESIAN_POINT('Ctrl Pts',(-1.28459209201807,0.199837668299145,
3.34673749165582));
#22815=CARTESIAN_POINT('Ctrl Pts',(-1.28373478569368,0.205,3.37421317147824));
#22816=CARTESIAN_POINT('Ctrl Pts',(-1.28373478569368,0.205,3.42578682852176));
#22817=CARTESIAN_POINT('Ctrl Pts',(-1.28459209201807,0.199837668299145,
3.45326250834418));
#22818=CARTESIAN_POINT('Ctrl Pts',(-1.2876744550022,0.178903418830812,3.50375720035387));
#22819=CARTESIAN_POINT('Ctrl Pts',(-1.28985344916615,0.163133809500307,
3.52677997078618));
#22820=CARTESIAN_POINT('Ctrl Pts',(-1.29393248914849,0.12678035877662,3.56313342150986));
#22821=CARTESIAN_POINT('Ctrl Pts',(-1.29609960028466,0.103757421316811,
3.57890333519745));
#22822=CARTESIAN_POINT('Ctrl Pts',(-1.29915469398922,0.0532621572488602,
3.59983780588318));
#22823=CARTESIAN_POINT('Ctrl Pts',(-1.3,0.025786278096092,3.605));
#22824=CARTESIAN_POINT('Ctrl Pts',(-1.3,1.17961196366423E-16,3.605));
#22825=CARTESIAN_POINT('Origin',(0.,-0.675,3.4));
#22826=CARTESIAN_POINT('',(0.203469899493758,-0.675,3.375));
#22827=CARTESIAN_POINT('',(0.203469899493758,-0.675,3.425));
#22828=CARTESIAN_POINT('',(0.203469899493758,-0.675,2.275));
#22829=CARTESIAN_POINT('Origin',(0.,-0.675,3.4));
#22830=CARTESIAN_POINT('Origin',(0.,-1.0025,3.4));
#22831=CARTESIAN_POINT('',(-2.29609705471212E-17,-0.705,3.195));
#22832=CARTESIAN_POINT('',(-2.51052593825207E-17,-1.0025,3.195));
#22833=CARTESIAN_POINT('',(-0.203469899493758,-0.675,3.375));
#22834=CARTESIAN_POINT('Ctrl Pts',(-0.203469899493758,-0.675,3.375));
#22835=CARTESIAN_POINT('Ctrl Pts',(-0.201242091014444,-0.675671543655374,
3.35686832130491));
#22836=CARTESIAN_POINT('Ctrl Pts',(-0.196469587434997,-0.67711148178717,
3.33857557904239));
#22837=CARTESIAN_POINT('Ctrl Pts',(-0.178826374035794,-0.682029730751166,
3.29611284356413));
#22838=CARTESIAN_POINT('Ctrl Pts',(-0.16307623613103,-0.68612968485916,
3.27316245584455));
#22839=CARTESIAN_POINT('Ctrl Pts',(-0.126842282640148,-0.693742502155627,
3.23692850235366));
#22840=CARTESIAN_POINT('Ctrl Pts',(-0.103889959828094,-0.697765433634744,
3.22117468990961));
#22841=CARTESIAN_POINT('Ctrl Pts',(-0.0534241842031802,-0.703431290629093,
3.20020642507842));
#22842=CARTESIAN_POINT('Ctrl Pts',(-0.0258990920208441,-0.705,3.195));
#22843=CARTESIAN_POINT('Ctrl Pts',(-6.93889390390723E-18,-0.705,3.195));
#22844=CARTESIAN_POINT('',(-0.203469899493758,-0.675,3.425));
#22845=CARTESIAN_POINT('Origin',(0.,-0.675,3.4));
#22846=CARTESIAN_POINT('Ctrl Pts',(0.203469899493758,-0.675,3.425));
#22847=CARTESIAN_POINT('Ctrl Pts',(0.201242091014444,-0.675671543655374,
3.44313167869509));
#22848=CARTESIAN_POINT('Ctrl Pts',(0.196469587434997,-0.677111481787171,
3.46142442095761));
#22849=CARTESIAN_POINT('Ctrl Pts',(0.178826374035794,-0.682029730751166,
3.50388715643587));
#22850=CARTESIAN_POINT('Ctrl Pts',(0.16307623613103,-0.68612968485916,3.52683754415545));
#22851=CARTESIAN_POINT('Ctrl Pts',(0.126842282640148,-0.693742502155627,
3.56307149764634));
#22852=CARTESIAN_POINT('Ctrl Pts',(0.103889959828094,-0.697765433634744,
3.57882531009039));
#22853=CARTESIAN_POINT('Ctrl Pts',(0.0534241842031802,-0.703431290629093,
3.59979357492158));
#22854=CARTESIAN_POINT('Ctrl Pts',(0.0258990920208441,-0.705,3.605));
#22855=CARTESIAN_POINT('Ctrl Pts',(-0.025899092020844,-0.705,3.605));
#22856=CARTESIAN_POINT('Ctrl Pts',(-0.0534241842031804,-0.703431290629093,
3.59979357492158));
#22857=CARTESIAN_POINT('Ctrl Pts',(-0.103889959828094,-0.697765433634744,
3.57882531009039));
#22858=CARTESIAN_POINT('Ctrl Pts',(-0.126842282640148,-0.693742502155627,
3.56307149764634));
#22859=CARTESIAN_POINT('Ctrl Pts',(-0.16307623613103,-0.68612968485916,
3.52683754415545));
#22860=CARTESIAN_POINT('Ctrl Pts',(-0.178826374035794,-0.682029730751166,
3.50388715643587));
#22861=CARTESIAN_POINT('Ctrl Pts',(-0.196469587434997,-0.67711148178717,
3.46142442095761));
#22862=CARTESIAN_POINT('Ctrl Pts',(-0.201242091014444,-0.675671543655374,
3.44313167869509));
#22863=CARTESIAN_POINT('Ctrl Pts',(-0.203469899493758,-0.675,3.425));
#22864=CARTESIAN_POINT('Ctrl Pts',(-2.08166817117217E-17,-0.705,3.195));
#22865=CARTESIAN_POINT('Ctrl Pts',(0.025899092020844,-0.705,3.195));
#22866=CARTESIAN_POINT('Ctrl Pts',(0.0534241842031803,-0.703431290629093,
3.20020642507842));
#22867=CARTESIAN_POINT('Ctrl Pts',(0.103889959828094,-0.697765433634744,
3.22117468990961));
#22868=CARTESIAN_POINT('Ctrl Pts',(0.126842282640148,-0.693742502155627,
3.23692850235366));
#22869=CARTESIAN_POINT('Ctrl Pts',(0.16307623613103,-0.68612968485916,3.27316245584455));
#22870=CARTESIAN_POINT('Ctrl Pts',(0.178826374035794,-0.682029730751166,
3.29611284356413));
#22871=CARTESIAN_POINT('Ctrl Pts',(0.196469587434997,-0.677111481787171,
3.33857557904239));
#22872=CARTESIAN_POINT('Ctrl Pts',(0.201242091014444,-0.675671543655374,
3.35686832130491));
#22873=CARTESIAN_POINT('Ctrl Pts',(0.203469899493758,-0.675,3.375));
#22874=CARTESIAN_POINT('Origin',(0.,-0.675,3.4));
#22875=CARTESIAN_POINT('',(-0.203469899493758,-0.675,2.275));
#22876=CARTESIAN_POINT('Origin',(0.95,0.,0.4));
#22877=CARTESIAN_POINT('',(-0.95,-1.16341445918999E-16,0.4));
#22878=CARTESIAN_POINT('Origin',(0.,0.,0.4));
#22879=CARTESIAN_POINT('Origin',(0.,0.,0.425));
#22880=CARTESIAN_POINT('',(-1.,-1.22464679914735E-16,0.45));
#22881=CARTESIAN_POINT('Origin',(0.,0.,0.45));
#22882=CARTESIAN_POINT('',(-0.975,-1.19403062916867E-16,0.425));
#22883=CARTESIAN_POINT('Origin',(0.,0.,1.625));
#22884=CARTESIAN_POINT('',(-1.,-1.22464679914735E-16,2.8));
#22885=CARTESIAN_POINT('Origin',(0.,0.,2.8));
#22886=CARTESIAN_POINT('',(-1.,-1.22464679914735E-16,1.625));
#22887=CARTESIAN_POINT('Origin',(1.25,0.,2.8));
#22888=CARTESIAN_POINT('',(-1.25,-1.53080849893419E-16,2.8));
#22889=CARTESIAN_POINT('Origin',(0.,0.,2.8));
#22890=CARTESIAN_POINT('Origin',(0.,0.,2.825));
#22891=CARTESIAN_POINT('',(-1.3,-1.59204083889156E-16,2.85));
#22892=CARTESIAN_POINT('Origin',(0.,0.,2.85));
#22893=CARTESIAN_POINT('',(-1.275,-1.56142466891288E-16,2.825));
#22894=CARTESIAN_POINT('Origin',(0.,0.,3.395));
#22895=CARTESIAN_POINT('',(-1.3,-1.59204083889156E-16,3.94));
#22896=CARTESIAN_POINT('Origin',(0.,0.,3.94));
#22897=CARTESIAN_POINT('',(-1.3,-1.59204083889156E-16,3.395));
#22898=CARTESIAN_POINT('',(-1.3,-1.59204083889156E-16,3.395));
#22899=CARTESIAN_POINT('Origin',(0.,0.,3.97));
#22900=CARTESIAN_POINT('',(-1.24,-1.51856203094272E-16,4.));
#22901=CARTESIAN_POINT('Origin',(0.,0.,4.));
#22902=CARTESIAN_POINT('',(-1.27,-1.55530143491714E-16,3.97));
#22903=CARTESIAN_POINT('Origin',(0.755,0.,4.));
#22904=CARTESIAN_POINT('',(-0.755,-9.24608333356252E-17,4.));
#22905=CARTESIAN_POINT('Origin',(0.,0.,4.));
#22906=CARTESIAN_POINT('Origin',(0.,0.,3.975));
#22907=CARTESIAN_POINT('',(-0.705,-8.63375993398884E-17,3.95));
#22908=CARTESIAN_POINT('',(-0.73,-8.93992163377568E-17,3.975));
#22909=CARTESIAN_POINT('Origin',(0.,0.,3.95));
#22910=CARTESIAN_POINT('Origin',(0.,0.,2.275));
#22911=CARTESIAN_POINT('',(-0.705,-8.63375993398884E-17,2.275));
#22912=CARTESIAN_POINT('',(-0.705,-8.63375993398884E-17,0.6));
#22913=CARTESIAN_POINT('',(-0.705,-8.63375993398884E-17,2.275));
#22914=CARTESIAN_POINT('Origin',(0.,0.,0.6));
#22915=CARTESIAN_POINT('Origin',(0.,0.,0.6));
#22916=CARTESIAN_POINT('',(0.,0.,0.));
#22917=CARTESIAN_POINT('Origin',(0.,-2.05499775283211E-17,6.0893933982822));
#22918=CARTESIAN_POINT('',(0.619999999999999,-7.59281015471358E-17,6.1));
#22919=CARTESIAN_POINT('Origin',(0.,0.,6.1));
#22920=CARTESIAN_POINT('',(0.671213203435596,8.21999101132844E-17,6.0787867965644));
#22921=CARTESIAN_POINT('',(0.645606601717798,7.90640058302101E-17,6.0893933982822));
#22922=CARTESIAN_POINT('',(-0.671213203435596,-8.21999101132843E-17,6.0787867965644));
#22923=CARTESIAN_POINT('Origin',(0.,-4.10999550566422E-17,6.0787867965644));
#22924=CARTESIAN_POINT('Origin',(0.,-4.10999550566422E-17,6.0787867965644));
#22925=CARTESIAN_POINT('Origin',(0.,0.,6.075));
#22926=CARTESIAN_POINT('',(-0.678786796564404,-8.31274077716083E-17,6.0712132034356));
#22927=CARTESIAN_POINT('',(-0.675,-8.26636589424463E-17,6.075));
#22928=CARTESIAN_POINT('',(0.678786796564404,-8.31274077716082E-17,6.0712132034356));
#22929=CARTESIAN_POINT('Origin',(0.,-4.15637038858041E-17,6.0712132034356));
#22930=CARTESIAN_POINT('Origin',(0.,-4.15637038858041E-17,6.0712132034356));
#22931=CARTESIAN_POINT('Origin',(0.,0.,6.1));
#22932=CARTESIAN_POINT('Origin',(0.,-2.07818519429021E-17,6.0456066017178));
#22933=CARTESIAN_POINT('',(0.7,8.57252759403147E-17,6.02));
#22934=CARTESIAN_POINT('',(0.689393398282202,8.44263418559615E-17,6.0456066017178));
#22935=CARTESIAN_POINT('',(-0.7,-8.57252759403147E-17,6.02));
#22936=CARTESIAN_POINT('Origin',(0.,0.,6.02));
#22937=CARTESIAN_POINT('Origin',(0.,0.,6.02));
#22938=CARTESIAN_POINT('Origin',(0.,0.,3.75));
#22939=CARTESIAN_POINT('',(-0.7,-8.57252759403147E-17,1.48));
#22940=CARTESIAN_POINT('',(-0.7,-8.57252759403147E-17,3.75));
#22941=CARTESIAN_POINT('',(0.7,-8.57252759403147E-17,1.48));
#22942=CARTESIAN_POINT('Origin',(0.,0.,1.48));
#22943=CARTESIAN_POINT('Origin',(0.,0.,1.48));
#22944=CARTESIAN_POINT('Origin',(0.,-2.07818519429021E-17,1.4543933982822));
#22945=CARTESIAN_POINT('',(0.678786796564404,8.31274077716083E-17,1.4287867965644));
#22946=CARTESIAN_POINT('',(0.689393398282202,8.44263418559615E-17,1.4543933982822));
#22947=CARTESIAN_POINT('',(-0.678786796564404,-8.31274077716083E-17,1.4287867965644));
#22948=CARTESIAN_POINT('Origin',(0.,-4.15637038858041E-17,1.4287867965644));
#22949=CARTESIAN_POINT('Origin',(0.,-4.15637038858041E-17,1.4287867965644));
#22950=CARTESIAN_POINT('Origin',(0.,0.,1.425));
#22951=CARTESIAN_POINT('',(-0.671213203435597,-8.21999101132845E-17,1.4212132034356));
#22952=CARTESIAN_POINT('',(-0.675,-8.26636589424463E-17,1.425));
#22953=CARTESIAN_POINT('',(0.671213203435597,-8.21999101132845E-17,1.4212132034356));
#22954=CARTESIAN_POINT('Origin',(0.,-4.10999550566422E-17,1.4212132034356));
#22955=CARTESIAN_POINT('Origin',(0.,-4.10999550566422E-17,1.4212132034356));
#22956=CARTESIAN_POINT('Origin',(0.,-2.05499775283211E-17,1.4106066017178));
#22957=CARTESIAN_POINT('',(0.62,7.59281015471359E-17,1.4));
#22958=CARTESIAN_POINT('',(0.645606601717798,7.90640058302102E-17,1.4106066017178));
#22959=CARTESIAN_POINT('Origin',(0.,0.,1.4));
#22960=CARTESIAN_POINT('Origin',(0.65,0.,1.4));
#22961=CARTESIAN_POINT('',(0.,0.,0.));
#22962=CARTESIAN_POINT('Origin',(2.7893933982822,-0.104393398282202,11.3));
#22963=CARTESIAN_POINT('',(2.78432776750217,-0.0921638837510863,6.44216388375109));
#22964=CARTESIAN_POINT('',(2.7787867965644,-0.0787867965644036,6.45));
#22965=CARTESIAN_POINT('',(2.39970611825836,0.836394918235631,6.98610103649399));
#22966=CARTESIAN_POINT('',(2.7787867965644,-0.0787867965644036,11.95));
#22967=CARTESIAN_POINT('',(2.7787867965644,-0.0787867965644035,11.3));
#22968=CARTESIAN_POINT('',(2.78432776750218,-0.092163883751089,11.9578361162489));
#22969=CARTESIAN_POINT('',(2.7349292673093,0.0270946453754314,11.8879760873153));
#22970=CARTESIAN_POINT('',(2.8,-0.13,11.92));
#22971=CARTESIAN_POINT('',(2.92207588469155,-0.424717256461034,11.625282743539));
#22972=CARTESIAN_POINT('',(2.8,-0.13,6.48));
#22973=CARTESIAN_POINT('',(2.8,-0.13,11.3));
#22974=CARTESIAN_POINT('',(3.32263738133569,-1.3917582542238,7.74175825422382));
#22975=CARTESIAN_POINT('Origin',(2.7893933982822,-0.85,11.9456066017178));
#22976=CARTESIAN_POINT('',(2.7787867965644,-0.1,11.9712132034356));
#22977=CARTESIAN_POINT('',(2.72691983628388,-0.173350958667782,12.0964311223839));
#22978=CARTESIAN_POINT('',(2.7787867965644,-0.8,11.9712132034356));
#22979=CARTESIAN_POINT('',(2.7787867965644,-0.85,11.9712132034356));
#22980=CARTESIAN_POINT('',(2.78757359312881,-0.812426406871192,11.95));
#22981=CARTESIAN_POINT('',(2.79216823850424,-0.818924216675421,11.9389075448203));
#22982=CARTESIAN_POINT('',(2.8,-0.8,11.92));
#22983=CARTESIAN_POINT('',(2.99252497643701,-0.607475023562985,11.4552035907902));
#22984=CARTESIAN_POINT('',(2.8,-0.85,11.92));
#22985=CARTESIAN_POINT('Origin',(2.8,-0.1,11.95));
#22986=CARTESIAN_POINT('',(2.7712132034356,-0.0712132034355967,11.95));
#22987=CARTESIAN_POINT('',(2.75,-0.0499999999999999,11.95));
#22988=CARTESIAN_POINT('',(2.75783611624891,-0.0656722324978244,11.9578361162489));
#22989=CARTESIAN_POINT('',(3.17114651601527,-0.2368710055509,11.7157244895356));
#22990=CARTESIAN_POINT('',(2.75,-0.0712132034355964,11.9712132034356));
#22991=CARTESIAN_POINT('',(2.37247760726871,-0.338161847385669,12.615684240117));
#22992=CARTESIAN_POINT('',(2.75,-0.0787867965644033,11.9787867965644));
#22993=CARTESIAN_POINT('',(2.75,-0.1,12.));
#22994=CARTESIAN_POINT('',(2.75783611624891,-0.0921638837510902,11.9843277675022));
#22995=CARTESIAN_POINT('',(2.21389896350601,0.836394918235626,11.5997061182584));
#22996=CARTESIAN_POINT('',(2.77121320343559,-0.1,11.9787867965644));
#22997=CARTESIAN_POINT('',(2.9197723149051,-0.187023912684747,11.9172515977796));
#22998=CARTESIAN_POINT('',(2.8,-0.1,11.95));
#22999=CARTESIAN_POINT('Origin',(2.775,-0.075,10.6));
#23000=CARTESIAN_POINT('',(2.7712132034356,-0.0712132034355967,6.45));
#23001=CARTESIAN_POINT('',(2.8,-0.1,6.45));
#23002=CARTESIAN_POINT('',(2.7712132034356,-0.0712132034355966,9.9));
#23003=CARTESIAN_POINT('Origin',(2.7893933982822,-0.85,6.4543933982822));
#23004=CARTESIAN_POINT('',(2.8,-0.8,6.48));
#23005=CARTESIAN_POINT('',(2.8,-0.85,6.48));
#23006=CARTESIAN_POINT('',(2.78757359312881,-0.812426406871193,6.45));
#23007=CARTESIAN_POINT('',(3.42427185655271,-0.175728143447283,7.98712558269742));
#23008=CARTESIAN_POINT('',(2.7787867965644,-0.8,6.4287867965644));
#23009=CARTESIAN_POINT('',(2.79216823850424,-0.818924216675423,6.46109245517966));
#23010=CARTESIAN_POINT('',(2.7787867965644,-0.1,6.4287867965644));
#23011=CARTESIAN_POINT('',(2.7787867965644,-0.85,6.4287867965644));
#23012=CARTESIAN_POINT('',(2.71725159777964,-0.187023912684737,6.2802276850949));
#23013=CARTESIAN_POINT('Origin',(2.8,-0.85,12.));
#23014=CARTESIAN_POINT('',(2.8,-0.8,10.6));
#23015=CARTESIAN_POINT('Origin',(2.75,-0.1,6.4));
#23016=CARTESIAN_POINT('',(2.7712132034356,-0.1,6.4212132034356));
#23017=CARTESIAN_POINT('',(2.75,-0.1,6.4));
#23018=CARTESIAN_POINT('',(2.75783611624891,-0.092163883751087,6.41567223249783));
#23019=CARTESIAN_POINT('',(2.8964311223839,-0.173350958667782,6.47308016371612));
#23020=CARTESIAN_POINT('',(2.75,-0.0787867965644033,6.4212132034356));
#23021=CARTESIAN_POINT('',(2.68797608731527,0.0270946453754293,6.4650707326907));
#23022=CARTESIAN_POINT('',(2.75,-0.0712132034355962,6.4287867965644));
#23023=CARTESIAN_POINT('',(2.75,-0.0499999999999999,6.45));
#23024=CARTESIAN_POINT('',(2.75783611624891,-0.0656722324978246,6.44216388375109));
#23025=CARTESIAN_POINT('',(2.51572448953563,-0.236871005550898,6.02885348398473));
#23026=CARTESIAN_POINT('',(3.41568424011697,-0.338161847385675,6.8275223927313));
#23027=CARTESIAN_POINT('Origin',(2.775,-0.825,10.6));
#23028=CARTESIAN_POINT('',(2.7712132034356,-0.828786796564403,11.95));
#23029=CARTESIAN_POINT('',(2.8,-0.8,11.95));
#23030=CARTESIAN_POINT('',(2.7712132034356,-0.828786796564403,6.45));
#23031=CARTESIAN_POINT('',(2.7712132034356,-0.828786796564403,9.9));
#23032=CARTESIAN_POINT('',(2.75,-0.85,6.45));
#23033=CARTESIAN_POINT('Origin',(2.75,-0.85,11.95));
#23034=CARTESIAN_POINT('',(2.77121320343559,-0.8,11.9787867965644));
#23035=CARTESIAN_POINT('',(2.75,-0.8,12.));
#23036=CARTESIAN_POINT('',(2.75783611624892,-0.80783611624891,11.9843277675022));
#23037=CARTESIAN_POINT('',(2.73890754482034,-0.818924216675422,11.9921682385042));
#23038=CARTESIAN_POINT('',(2.75,-0.821213203435597,11.9787867965644));
#23039=CARTESIAN_POINT('',(2.19856720201026,-1.76256787225257,11.5888649257372));
#23040=CARTESIAN_POINT('',(2.75,-0.828786796564404,11.9712132034356));
#23041=CARTESIAN_POINT('',(2.75,-0.85,11.95));
#23042=CARTESIAN_POINT('',(2.75783611624891,-0.834327767502176,11.9578361162489));
#23043=CARTESIAN_POINT('',(2.3708187997899,-0.56066519859738,12.6185160016127));
#23044=CARTESIAN_POINT('',(3.14780532349409,-0.672797232953338,11.7293974435526));
#23045=CARTESIAN_POINT('Origin',(2.1,-0.104393398282202,6.4106066017178));
#23046=CARTESIAN_POINT('',(-2.75783611624891,-0.0921638837510879,6.41567223249783));
#23047=CARTESIAN_POINT('',(-2.75,-0.0787867965644033,6.4212132034356));
#23048=CARTESIAN_POINT('',(-2.21389896350603,0.836394918235614,6.80029388174163));
#23049=CARTESIAN_POINT('',(2.1,-0.0787867965644035,6.4212132034356));
#23050=CARTESIAN_POINT('',(2.72,-0.13,6.4));
#23051=CARTESIAN_POINT('',(2.42528274353897,-0.424717256461035,6.27792411530845));
#23052=CARTESIAN_POINT('',(-2.72,-0.13,6.4));
#23053=CARTESIAN_POINT('',(2.1,-0.13,6.4));
#23054=CARTESIAN_POINT('',(-1.45824174577622,-1.3917582542238,5.8773626186643));
#23055=CARTESIAN_POINT('Origin',(-2.7456066017178,-0.85,6.4106066017178));
#23056=CARTESIAN_POINT('',(-2.72,-0.769999999999999,6.4));
#23057=CARTESIAN_POINT('',(-2.72,-0.85,6.4));
#23058=CARTESIAN_POINT('',(-2.75783611624891,-0.807836116248913,6.41567223249782));
#23059=CARTESIAN_POINT('',(-1.64244003106437,0.30755996893565,5.95366004659652));
#23060=CARTESIAN_POINT('',(-2.7712132034356,-0.8,6.4212132034356));
#23061=CARTESIAN_POINT('',(-2.73890754482034,-0.818924216675422,6.40783176149576));
#23062=CARTESIAN_POINT('',(-2.7712132034356,-0.1,6.4212132034356));
#23063=CARTESIAN_POINT('',(-2.7712132034356,-0.85,6.4212132034356));
#23064=CARTESIAN_POINT('',(-2.9197723149051,-0.187023912684738,6.48274840222036));
#23065=CARTESIAN_POINT('Origin',(2.8,-0.85,6.4));
#23066=CARTESIAN_POINT('',(2.72,-0.769999999999999,6.4));
#23067=CARTESIAN_POINT('',(2.72,-0.85,6.4));
#23068=CARTESIAN_POINT('',(2.1,-0.769999999999999,6.4));
#23069=CARTESIAN_POINT('Origin',(2.7456066017178,-0.85,6.4106066017178));
#23070=CARTESIAN_POINT('',(2.7712132034356,-0.8,6.4212132034356));
#23071=CARTESIAN_POINT('',(2.7712132034356,-0.85,6.4212132034356));
#23072=CARTESIAN_POINT('',(2.75783611624891,-0.807836116248912,6.41567223249782));
#23073=CARTESIAN_POINT('',(2.73890754482034,-0.818924216675421,6.40783176149576));
#23074=CARTESIAN_POINT('',(2.60948102882711,-0.659481028827113,6.35422154324067));
#23075=CARTESIAN_POINT('Origin',(1.4,-0.075,6.425));
#23076=CARTESIAN_POINT('',(-2.75,-0.0712132034355962,6.4287867965644));
#23077=CARTESIAN_POINT('',(-2.75,-0.1,6.4));
#23078=CARTESIAN_POINT('',(0.7,-0.0712132034355964,6.4287867965644));
#23079=CARTESIAN_POINT('Origin',(-2.8,-0.1,6.45));
#23080=CARTESIAN_POINT('',(-2.7787867965644,-0.1,6.4287867965644));
#23081=CARTESIAN_POINT('',(-2.8,-0.1,6.45));
#23082=CARTESIAN_POINT('',(-2.78432776750217,-0.0921638837510875,6.44216388375109));
#23083=CARTESIAN_POINT('',(-2.72691983628388,-0.173350958667781,6.3035688776161));
#23084=CARTESIAN_POINT('',(-2.7787867965644,-0.0787867965644036,6.45));
#23085=CARTESIAN_POINT('',(-2.73492926730931,0.0270946453754293,6.51202391268473));
#23086=CARTESIAN_POINT('',(-2.7712132034356,-0.0712132034355967,6.45));
#23087=CARTESIAN_POINT('',(-2.75,-0.0499999999999999,6.45));
#23088=CARTESIAN_POINT('',(-2.75783611624891,-0.0656722324978246,6.44216388375109));
#23089=CARTESIAN_POINT('',(-3.17114651601528,-0.236871005550901,6.68427551046438));
#23090=CARTESIAN_POINT('',(-2.37247760726871,-0.338161847385672,5.78431575988303));
#23091=CARTESIAN_POINT('Origin',(-2.7893933982822,-0.104393398282202,7.1));
#23092=CARTESIAN_POINT('',(-2.78432776750218,-0.0921638837510882,11.9578361162489));
#23093=CARTESIAN_POINT('',(-2.7787867965644,-0.0787867965644036,11.95));
#23094=CARTESIAN_POINT('',(-2.39970611825836,0.836394918235639,11.413898963506));
#23095=CARTESIAN_POINT('',(-2.7787867965644,-0.0787867965644035,7.1));
#23096=CARTESIAN_POINT('',(-2.8,-0.13,6.48));
#23097=CARTESIAN_POINT('',(-2.92207588469155,-0.424717256461036,6.77471725646103));
#23098=CARTESIAN_POINT('',(-2.8,-0.13,11.92));
#23099=CARTESIAN_POINT('',(-2.8,-0.13,7.1));
#23100=CARTESIAN_POINT('',(-3.3226373813357,-1.3917582542238,10.6582417457763));
#23101=CARTESIAN_POINT('Origin',(-2.7893933982822,-0.85,11.9456066017178));
#23102=CARTESIAN_POINT('',(-2.8,-0.8,11.92));
#23103=CARTESIAN_POINT('',(-2.8,-0.85,11.92));
#23104=CARTESIAN_POINT('',(-2.78757359312881,-0.812426406871193,11.95));
#23105=CARTESIAN_POINT('',(-3.42427185655274,-0.175728143447254,10.4128744173027));
#23106=CARTESIAN_POINT('',(-2.7787867965644,-0.8,11.9712132034356));
#23107=CARTESIAN_POINT('',(-2.78132704598305,-0.803592455179658,11.9650804988373));
#23108=CARTESIAN_POINT('',(-2.7787867965644,-0.1,11.9712132034356));
#23109=CARTESIAN_POINT('',(-2.7787867965644,-0.85,11.9712132034356));
#23110=CARTESIAN_POINT('',(-2.71725159777964,-0.187023912684724,12.1197723149051));
#23111=CARTESIAN_POINT('Origin',(-2.8,-0.85,6.4));
#23112=CARTESIAN_POINT('',(-2.8,-0.8,6.48));
#23113=CARTESIAN_POINT('',(-2.8,-0.85,6.48));
#23114=CARTESIAN_POINT('',(-2.8,-0.8,7.8));
#23115=CARTESIAN_POINT('Origin',(-2.7893933982822,-0.85,6.4543933982822));
#23116=CARTESIAN_POINT('',(-2.7787867965644,-0.8,6.4287867965644));
#23117=CARTESIAN_POINT('',(-2.7787867965644,-0.85,6.4287867965644));
#23118=CARTESIAN_POINT('',(-2.78757359312881,-0.812426406871193,6.45));
#23119=CARTESIAN_POINT('',(-2.79216823850424,-0.818924216675421,6.46109245517966));
#23120=CARTESIAN_POINT('',(-2.99252497643702,-0.607475023562983,6.9447964092098));
#23121=CARTESIAN_POINT('Origin',(-2.775,-0.825,7.8));
#23122=CARTESIAN_POINT('',(-2.7712132034356,-0.828786796564403,6.45));
#23123=CARTESIAN_POINT('',(-2.8,-0.8,6.45));
#23124=CARTESIAN_POINT('',(-2.7712132034356,-0.828786796564403,11.95));
#23125=CARTESIAN_POINT('',(-2.7712132034356,-0.828786796564403,8.5));
#23126=CARTESIAN_POINT('',(-2.75,-0.85,11.95));
#23127=CARTESIAN_POINT('Origin',(-2.75,-0.85,6.45));
#23128=CARTESIAN_POINT('',(-2.75,-0.821213203435597,6.4212132034356));
#23129=CARTESIAN_POINT('',(-2.19856720201027,-1.76256787225257,6.81113507426282));
#23130=CARTESIAN_POINT('',(-2.75,-0.828786796564403,6.4287867965644));
#23131=CARTESIAN_POINT('',(-2.75,-0.85,6.45));
#23132=CARTESIAN_POINT('',(-2.75783611624891,-0.834327767502175,6.44216388375109));
#23133=CARTESIAN_POINT('',(-2.37081879978991,-0.560665198597375,5.78148399838728));
#23134=CARTESIAN_POINT('',(-3.14780532349409,-0.672797232953337,6.67060255644743));
#23135=CARTESIAN_POINT('',(-2.75,-0.8,6.4));
#23136=CARTESIAN_POINT('Origin',(-2.75,-0.1,12.));
#23137=CARTESIAN_POINT('',(-2.77121320343559,-0.1,11.9787867965644));
#23138=CARTESIAN_POINT('',(-2.75,-0.1,12.));
#23139=CARTESIAN_POINT('',(-2.75783611624891,-0.0921638837510905,11.9843277675022));
#23140=CARTESIAN_POINT('',(-2.89643112238391,-0.173350958667796,11.9269198362839));
#23141=CARTESIAN_POINT('',(-2.75,-0.0787867965644033,11.9787867965644));
#23142=CARTESIAN_POINT('',(-2.68797608731526,0.027094645375429,11.9349292673093));
#23143=CARTESIAN_POINT('',(-2.75,-0.0712132034355964,11.9712132034356));
#23144=CARTESIAN_POINT('',(-2.75,-0.0499999999999999,11.95));
#23145=CARTESIAN_POINT('',(-2.75783611624891,-0.0656722324978241,11.9578361162489));
#23146=CARTESIAN_POINT('',(-2.51572448953563,-0.236871005550895,12.3711465160153));
#23147=CARTESIAN_POINT('',(-2.7712132034356,-0.0712132034355967,11.95));
#23148=CARTESIAN_POINT('',(-3.41568424011698,-0.338161847385678,11.5724776072687));
#23149=CARTESIAN_POINT('',(-2.8,-0.1,11.95));
#23150=CARTESIAN_POINT('Origin',(-2.775,-0.85,11.975));
#23151=CARTESIAN_POINT('',(-2.77121320343559,-0.8,11.9787867965644));
#23152=CARTESIAN_POINT('',(-2.8,-0.8,11.95));
#23153=CARTESIAN_POINT('',(-2.7712132034356,-0.85,11.9787867965644));
#23154=CARTESIAN_POINT('Origin',(-2.75,-0.8,12.));
#23155=CARTESIAN_POINT('',(-2.75783611624891,-0.834327767502176,11.9578361162489));
#23156=CARTESIAN_POINT('',(-3.41568424011698,-0.561838152614322,11.5724776072687));
#23157=CARTESIAN_POINT('',(-2.75,-0.828786796564404,11.9712132034356));
#23158=CARTESIAN_POINT('',(-2.51572448953563,-0.663128994449105,12.3711465160153));
#23159=CARTESIAN_POINT('',(-2.75,-0.821213203435597,11.9787867965644));
#23160=CARTESIAN_POINT('',(-2.75,-0.8,12.));
#23161=CARTESIAN_POINT('',(-2.75783611624891,-0.80783611624891,11.9843277675022));
#23162=CARTESIAN_POINT('',(-2.68797608731526,-0.927094645375429,11.9349292673093));
#23163=CARTESIAN_POINT('',(-2.7417393063161,-0.817265409196609,11.9909952844873));
#23164=CARTESIAN_POINT('Origin',(-2.1,-0.104393398282201,11.9893933982822));
#23165=CARTESIAN_POINT('',(-2.1,-0.0787867965644031,11.9787867965644));
#23166=CARTESIAN_POINT('',(-2.72,-0.129999999999999,12.));
#23167=CARTESIAN_POINT('',(-2.42528274353895,-0.42471725646102,12.1220758846915));
#23168=CARTESIAN_POINT('',(2.72,-0.129999999999999,12.));
#23169=CARTESIAN_POINT('',(-2.1,-0.129999999999999,12.));
#23170=CARTESIAN_POINT('',(1.4582417457761,-1.39175825422379,12.5226373813357));
#23171=CARTESIAN_POINT('Origin',(-2.7456066017178,-0.85,11.9893933982822));
#23172=CARTESIAN_POINT('',(-2.72,-0.770000000000001,12.));
#23173=CARTESIAN_POINT('',(-2.6094810288271,-0.659481028827109,12.0457784567593));
#23174=CARTESIAN_POINT('',(-2.72,-0.85,12.));
#23175=CARTESIAN_POINT('Origin',(-1.4,-0.075,11.975));
#23176=CARTESIAN_POINT('',(-0.7,-0.0712132034355963,11.9712132034356));
#23177=CARTESIAN_POINT('Origin',(2.7456066017178,-0.85,11.9893933982822));
#23178=CARTESIAN_POINT('',(2.72,-0.770000000000001,12.));
#23179=CARTESIAN_POINT('',(2.72,-0.85,12.));
#23180=CARTESIAN_POINT('',(1.64244003106424,0.307559968935658,12.4463399534035));
#23181=CARTESIAN_POINT('',(2.77121320343559,-0.85,11.9787867965644));
#23182=CARTESIAN_POINT('Origin',(-2.1,-0.795606601717799,11.9893933982822));
#23183=CARTESIAN_POINT('',(-2.1,-0.770000000000001,12.));
#23184=CARTESIAN_POINT('',(-2.1,-0.821213203435597,11.9787867965644));
#23185=CARTESIAN_POINT('Origin',(-2.8,-0.85,12.));
#23186=CARTESIAN_POINT('Origin',(-2.7456066017178,-0.0606066017177983,8.5));
#23187=CARTESIAN_POINT('',(-2.7712132034356,-0.0712132034355966,8.5));
#23188=CARTESIAN_POINT('',(-2.72,-0.0499999999999999,11.92));
#23189=CARTESIAN_POINT('',(-1.48126653143723,0.463100202844175,10.6812665314372));
#23190=CARTESIAN_POINT('',(-2.72,-0.0499999999999999,6.48));
#23191=CARTESIAN_POINT('',(-2.72,-0.0499999999999999,8.5));
#23192=CARTESIAN_POINT('',(-1.48126653143723,0.463100202844175,7.71873346856278));
#23193=CARTESIAN_POINT('Origin',(-0.7,-0.0606066017177981,11.9456066017178));
#23194=CARTESIAN_POINT('',(2.72,-0.0499999999999999,11.92));
#23195=CARTESIAN_POINT('',(1.48126653143723,0.463100202844174,10.6812665314372));
#23196=CARTESIAN_POINT('',(-0.7,-0.0499999999999999,11.92));
#23197=CARTESIAN_POINT('Origin',(-2.775,-0.075,7.8));
#23198=CARTESIAN_POINT('Origin',(2.7456066017178,-0.0606066017177983,9.9));
#23199=CARTESIAN_POINT('',(2.72,-0.0499999999999999,6.48));
#23200=CARTESIAN_POINT('',(1.48126653143723,0.463100202844176,7.71873346856278));
#23201=CARTESIAN_POINT('',(2.72,-0.0499999999999999,9.9));
#23202=CARTESIAN_POINT('Origin',(0.,-0.0499999999999999,9.2));
#23203=CARTESIAN_POINT('',(0.7,-0.0499999999999999,6.48));
#23204=CARTESIAN_POINT('',(1.7,-0.0499999999999999,9.745));
#23205=CARTESIAN_POINT('Origin',(1.7,-0.0499999999999999,10.));
#23206=CARTESIAN_POINT('',(-2.,-0.0499999999999999,7.015));
#23207=CARTESIAN_POINT('Origin',(-2.,-0.0499999999999999,7.3));
#23208=CARTESIAN_POINT('',(2.,-0.0499999999999999,7.015));
#23209=CARTESIAN_POINT('Origin',(2.,-0.0499999999999999,7.3));
#23210=CARTESIAN_POINT('',(2.,-0.0499999999999999,10.815));
#23211=CARTESIAN_POINT('Origin',(2.,-0.0499999999999999,11.1));
#23212=CARTESIAN_POINT('',(-3.12284933782576E-17,-0.0499999999999999,7.045));
#23213=CARTESIAN_POINT('Origin',(0.,-0.0499999999999999,7.3));
#23214=CARTESIAN_POINT('',(-1.785,-0.0499999999999999,9.7));
#23215=CARTESIAN_POINT('Origin',(-0.4,-0.0499999999999999,9.7));
#23216=CARTESIAN_POINT('Origin',(0.7,-0.0606066017177982,6.4543933982822));
#23217=CARTESIAN_POINT('Origin',(-1.4,-0.825,11.975));
#23218=CARTESIAN_POINT('',(-0.7,-0.828786796564404,11.9712132034356));
#23219=CARTESIAN_POINT('Origin',(2.1,-0.795606601717798,6.4106066017178));
#23220=CARTESIAN_POINT('',(2.75,-0.821213203435597,6.4212132034356));
#23221=CARTESIAN_POINT('',(2.67430313329832,-0.950435837896618,6.47473897119493));
#23222=CARTESIAN_POINT('',(2.1,-0.821213203435596,6.4212132034356));
#23223=CARTESIAN_POINT('Origin',(1.4,-0.825,6.425));
#23224=CARTESIAN_POINT('',(2.75,-0.828786796564403,6.4287867965644));
#23225=CARTESIAN_POINT('',(2.75,-0.8,6.4));
#23226=CARTESIAN_POINT('',(0.7,-0.828786796564403,6.4287867965644));
#23227=CARTESIAN_POINT('Origin',(2.75,-0.85,6.45));
#23228=CARTESIAN_POINT('',(2.75783611624891,-0.834327767502175,6.44216388375109));
#23229=CARTESIAN_POINT('',(3.41851600161273,-0.560665198597375,6.82918120021011));
#23230=CARTESIAN_POINT('',(2.52939744355258,-0.672797232953338,6.05219467650592));
#23231=CARTESIAN_POINT('',(2.8,-0.8,6.45));
#23232=CARTESIAN_POINT('Origin',(-0.4,-0.795606601717798,9.7));
#23233=CARTESIAN_POINT('',(0.7,-0.77,9.7));
#23234=CARTESIAN_POINT('',(-1.5,-0.77,9.7));
#23235=CARTESIAN_POINT('Origin',(-0.4,-0.77,9.7));
#23236=CARTESIAN_POINT('Origin',(-0.4,-0.77,9.7));
#23237=CARTESIAN_POINT('',(0.721213203435596,-0.821213203435596,9.7));
#23238=CARTESIAN_POINT('',(0.710606601717798,-0.795606601717798,9.7));
#23239=CARTESIAN_POINT('',(-1.5212132034356,-0.821213203435596,9.7));
#23240=CARTESIAN_POINT('Origin',(-0.4,-0.821213203435596,9.7));
#23241=CARTESIAN_POINT('Origin',(-0.4,-0.821213203435596,9.7));
#23242=CARTESIAN_POINT('Origin',(-0.4,-0.75,9.7));
#23243=CARTESIAN_POINT('',(0.7,-0.73,9.7));
#23244=CARTESIAN_POINT('',(-1.5,-0.73,9.7));
#23245=CARTESIAN_POINT('Origin',(-0.4,-0.73,9.7));
#23246=CARTESIAN_POINT('Origin',(-0.4,-0.73,9.7));
#23247=CARTESIAN_POINT('',(-1.5,-0.75,9.7));
#23248=CARTESIAN_POINT('Origin',(-0.4,-0.84,9.7));
#23249=CARTESIAN_POINT('',(-1.5287867965644,-0.828786796564404,9.7));
#23250=CARTESIAN_POINT('',(-1.54,-0.84,9.7));
#23251=CARTESIAN_POINT('Origin',(-0.4,-0.828786796564404,9.7));
#23252=CARTESIAN_POINT('Origin',(-0.4,-0.715,9.7));
#23253=CARTESIAN_POINT('',(0.73,-0.7,9.7));
#23254=CARTESIAN_POINT('Origin',(-0.4,-0.7,9.7));
#23255=CARTESIAN_POINT('',(0.715,-0.715,9.7));
#23256=CARTESIAN_POINT('Origin',(0.7,-0.7,9.7));
#23257=CARTESIAN_POINT('',(-1.66,-0.7,9.7));
#23258=CARTESIAN_POINT('Origin',(-0.4,-0.7,9.7));
#23259=CARTESIAN_POINT('Origin',(-0.4,-0.415,9.7));
#23260=CARTESIAN_POINT('',(0.89,-0.4,9.7));
#23261=CARTESIAN_POINT('Origin',(-0.4,-0.4,9.7));
#23262=CARTESIAN_POINT('',(0.86,-0.43,9.7));
#23263=CARTESIAN_POINT('',(0.875,-0.415,9.7));
#23264=CARTESIAN_POINT('',(-1.66,-0.43,9.7));
#23265=CARTESIAN_POINT('Origin',(-0.4,-0.43,9.7));
#23266=CARTESIAN_POINT('Origin',(-0.4,-0.43,9.7));
#23267=CARTESIAN_POINT('Origin',(0.86,-0.4,9.7));
#23268=CARTESIAN_POINT('',(-1.755,-0.4,9.7));
#23269=CARTESIAN_POINT('Origin',(-0.4,-0.4,9.7));
#23270=CARTESIAN_POINT('Origin',(-0.4,-0.55,9.7));
#23271=CARTESIAN_POINT('',(-1.66,-0.55,9.7));
#23272=CARTESIAN_POINT('Origin',(-0.4,-0.0649999999999999,9.7));
#23273=CARTESIAN_POINT('',(-1.755,-0.0799999999999999,9.7));
#23274=CARTESIAN_POINT('',(-1.77,-0.0649999999999999,9.7));
#23275=CARTESIAN_POINT('Origin',(-0.4,-0.0799999999999999,9.7));
#23276=CARTESIAN_POINT('Origin',(-0.4,-0.21,9.7));
#23277=CARTESIAN_POINT('',(-1.755,-0.21,9.7));
#23278=CARTESIAN_POINT('Origin',(1.7,-0.0649999999999999,10.));
#23279=CARTESIAN_POINT('',(1.7,-0.0799999999999999,9.775));
#23280=CARTESIAN_POINT('',(1.7,-0.0649999999999999,9.76));
#23281=CARTESIAN_POINT('Origin',(1.7,-0.0799999999999999,10.));
#23282=CARTESIAN_POINT('Origin',(1.7,-0.135,10.));
#23283=CARTESIAN_POINT('',(1.7,-0.22,10.225));
#23284=CARTESIAN_POINT('',(1.7,-0.22,9.775));
#23285=CARTESIAN_POINT('Origin',(1.7,-0.22,10.));
#23286=CARTESIAN_POINT('Origin',(1.7,-0.22,10.));
#23287=CARTESIAN_POINT('',(1.7,-0.135,9.775));
#23288=CARTESIAN_POINT('Origin',(1.7,-0.235,10.));
#23289=CARTESIAN_POINT('',(1.7,-0.25,10.255));
#23290=CARTESIAN_POINT('Origin',(1.7,-0.25,10.));
#23291=CARTESIAN_POINT('',(1.7,-0.235,10.24));
#23292=CARTESIAN_POINT('Origin',(1.7,-0.25,10.225));
#23293=CARTESIAN_POINT('',(1.7,-0.25,9.6));
#23294=CARTESIAN_POINT('Origin',(1.7,-0.25,10.));
#23295=CARTESIAN_POINT('Origin',(0.,-0.0649999999999999,7.3));
#23296=CARTESIAN_POINT('',(2.75545529808155E-17,-0.0799999999999999,7.075));
#23297=CARTESIAN_POINT('',(-2.93915231795366E-17,-0.0649999999999999,7.06));
#23298=CARTESIAN_POINT('Origin',(0.,-0.0799999999999999,7.3));
#23299=CARTESIAN_POINT('Origin',(0.,-0.135,7.3));
#23300=CARTESIAN_POINT('',(2.75545529808155E-17,-0.22,7.525));
#23301=CARTESIAN_POINT('',(-2.75545529808155E-17,-0.22,7.075));
#23302=CARTESIAN_POINT('Origin',(0.,-0.22,7.3));
#23303=CARTESIAN_POINT('Origin',(0.,-0.22,7.3));
#23304=CARTESIAN_POINT('',(-2.75545529808155E-17,-0.135,7.075));
#23305=CARTESIAN_POINT('Origin',(0.,-0.235,7.3));
#23306=CARTESIAN_POINT('',(-3.12284933782576E-17,-0.25,7.555));
#23307=CARTESIAN_POINT('Origin',(0.,-0.25,7.3));
#23308=CARTESIAN_POINT('',(-2.93915231795366E-17,-0.235,7.54));
#23309=CARTESIAN_POINT('Origin',(0.,-0.25,7.525));
#23310=CARTESIAN_POINT('',(-4.89858719658942E-17,-0.25,6.9));
#23311=CARTESIAN_POINT('Origin',(0.,-0.25,7.3));
#23312=CARTESIAN_POINT('Origin',(-2.,-0.0649999999999999,7.3));
#23313=CARTESIAN_POINT('',(-2.,-0.08,7.045));
#23314=CARTESIAN_POINT('',(-2.,-0.0649999999999999,7.03));
#23315=CARTESIAN_POINT('Origin',(-2.,-0.08,7.3));
#23316=CARTESIAN_POINT('Origin',(-2.,-0.45,7.3));
#23317=CARTESIAN_POINT('',(-2.,-0.82,7.045));
#23318=CARTESIAN_POINT('Origin',(-2.,-0.82,7.3));
#23319=CARTESIAN_POINT('',(-2.,-0.45,7.045));
#23320=CARTESIAN_POINT('Origin',(2.,-0.0649999999999999,11.1));
#23321=CARTESIAN_POINT('',(2.,-0.08,10.845));
#23322=CARTESIAN_POINT('',(2.,-0.0649999999999999,10.83));
#23323=CARTESIAN_POINT('Origin',(2.,-0.08,11.1));
#23324=CARTESIAN_POINT('Origin',(2.,-0.45,11.1));
#23325=CARTESIAN_POINT('',(2.,-0.82,10.845));
#23326=CARTESIAN_POINT('Origin',(2.,-0.82,11.1));
#23327=CARTESIAN_POINT('',(2.,-0.45,10.845));
#23328=CARTESIAN_POINT('Origin',(2.,-0.0649999999999999,7.3));
#23329=CARTESIAN_POINT('',(2.,-0.08,7.045));
#23330=CARTESIAN_POINT('',(2.,-0.0649999999999999,7.03));
#23331=CARTESIAN_POINT('Origin',(2.,-0.08,7.3));
#23332=CARTESIAN_POINT('Origin',(2.,-0.45,7.3));
#23333=CARTESIAN_POINT('',(2.,-0.82,7.045));
#23334=CARTESIAN_POINT('Origin',(2.,-0.82,7.3));
#23335=CARTESIAN_POINT('',(2.,-0.45,7.045));
#23336=CARTESIAN_POINT('Origin',(0.,-0.835,7.3));
#23337=CARTESIAN_POINT('',(5.26598123633363E-17,-0.85,6.87));
#23338=CARTESIAN_POINT('Origin',(0.,-0.85,7.3));
#23339=CARTESIAN_POINT('',(-4.89858719658942E-17,-0.82,6.9));
#23340=CARTESIAN_POINT('',(5.08228421646152E-17,-0.835,6.885));
#23341=CARTESIAN_POINT('Origin',(0.,-0.82,7.3));
#23342=CARTESIAN_POINT('Origin',(0.,-0.85,9.2));
#23343=CARTESIAN_POINT('',(2.72,-0.85,11.92));
#23344=CARTESIAN_POINT('',(2.72,-0.85,6.48));
#23345=CARTESIAN_POINT('',(2.72,-0.85,9.9));
#23346=CARTESIAN_POINT('',(-2.72,-0.85,11.92));
#23347=CARTESIAN_POINT('',(-0.7,-0.85,11.92));
#23348=CARTESIAN_POINT('',(-2.72,-0.85,6.48));
#23349=CARTESIAN_POINT('',(-2.72,-0.85,8.5));
#23350=CARTESIAN_POINT('',(0.7,-0.85,6.48));
#23351=CARTESIAN_POINT('',(1.7,-0.85,9.57));
#23352=CARTESIAN_POINT('Origin',(1.7,-0.85,10.));
#23353=CARTESIAN_POINT('',(2.,-0.85,7.015));
#23354=CARTESIAN_POINT('Origin',(2.,-0.85,7.3));
#23355=CARTESIAN_POINT('',(-2.,-0.85,7.015));
#23356=CARTESIAN_POINT('Origin',(-2.,-0.85,7.3));
#23357=CARTESIAN_POINT('',(2.,-0.85,10.815));
#23358=CARTESIAN_POINT('Origin',(2.,-0.85,11.1));
#23359=CARTESIAN_POINT('',(-1.58,-0.85,9.7));
#23360=CARTESIAN_POINT('Origin',(-0.4,-0.85,9.7));
#23361=CARTESIAN_POINT('Origin',(0.,-0.565,7.3));
#23362=CARTESIAN_POINT('',(-4.89858719658942E-17,-0.565,6.9));
#23363=CARTESIAN_POINT('Origin',(1.7,-0.835,10.));
#23364=CARTESIAN_POINT('',(1.7,-0.82,9.6));
#23365=CARTESIAN_POINT('',(1.7,-0.835,9.585));
#23366=CARTESIAN_POINT('Origin',(1.7,-0.82,10.));
#23367=CARTESIAN_POINT('Origin',(1.7,-0.565,10.));
#23368=CARTESIAN_POINT('',(1.7,-0.565,9.6));
#23369=CARTESIAN_POINT('Origin',(-0.4,-0.839393398282202,9.7));
#23370=CARTESIAN_POINT('',(-1.5543933982822,-0.839393398282202,9.7));
#23371=CARTESIAN_POINT('Origin',(2.7456066017178,-0.839393398282202,9.9));
#23372=CARTESIAN_POINT('',(1.48126653143723,-1.36310020284417,10.6812665314372));
#23373=CARTESIAN_POINT('',(1.48126653143722,-1.36310020284418,7.71873346856276));
#23374=CARTESIAN_POINT('Origin',(-0.7,-0.839393398282202,11.9456066017178));
#23375=CARTESIAN_POINT('',(-1.48126653143723,-1.36310020284417,10.6812665314372));
#23376=CARTESIAN_POINT('Origin',(-2.7456066017178,-0.839393398282202,8.5));
#23377=CARTESIAN_POINT('',(-1.48126653143721,-1.36310020284418,7.71873346856277));
#23378=CARTESIAN_POINT('Origin',(0.7,-0.839393398282201,6.4543933982822));
#23379=CARTESIAN_POINT('Origin',(2.,-0.835,7.3));
#23380=CARTESIAN_POINT('',(2.,-0.835,7.03));
#23381=CARTESIAN_POINT('Origin',(2.,-0.835,11.1));
#23382=CARTESIAN_POINT('',(2.,-0.835,10.83));
#23383=CARTESIAN_POINT('Origin',(-2.,-0.835,7.3));
#23384=CARTESIAN_POINT('',(-2.,-0.835,7.03));
#23385=CARTESIAN_POINT('Origin',(-2.775,-0.85,6.425));
#23386=CARTESIAN_POINT('Origin',(2.775,-0.85,11.975));
#23387=CARTESIAN_POINT('Origin',(2.775,-0.85,6.425));
#23388=CARTESIAN_POINT('',(0.,0.,0.));
#23389=CARTESIAN_POINT('Origin',(0.82,-0.4,9.7));
#23390=CARTESIAN_POINT('',(-1.62,-0.4,9.7));
#23391=CARTESIAN_POINT('Origin',(-0.4,-0.4,9.7));
#23392=CARTESIAN_POINT('Origin',(-0.4,-0.415,9.7));
#23393=CARTESIAN_POINT('',(-1.65,-0.43,9.7));
#23394=CARTESIAN_POINT('Origin',(-0.4,-0.43,9.7));
#23395=CARTESIAN_POINT('',(-1.635,-0.415,9.7));
#23396=CARTESIAN_POINT('Origin',(-0.4,-0.55,9.7));
#23397=CARTESIAN_POINT('',(-1.65,-0.67,9.7));
#23398=CARTESIAN_POINT('Origin',(-0.4,-0.67,9.7));
#23399=CARTESIAN_POINT('',(-1.65,-0.55,9.7));
#23400=CARTESIAN_POINT('Origin',(-0.4,-0.685,9.7));
#23401=CARTESIAN_POINT('',(-1.62,-0.7,9.7));
#23402=CARTESIAN_POINT('Origin',(-0.4,-0.7,9.7));
#23403=CARTESIAN_POINT('',(-1.635,-0.685,9.7));
#23404=CARTESIAN_POINT('Origin',(-0.4,-0.7,9.7));
#23405=CARTESIAN_POINT('',(0.,0.,0.));
#23406=CARTESIAN_POINT('Origin',(-0.4,-0.255,9.7));
#23407=CARTESIAN_POINT('',(-1.74415870087061,-0.266244406628447,9.70002284206962));
#23408=CARTESIAN_POINT('',(-1.74424829702886,-0.252155593372042,9.70002193782831));
#23409=CARTESIAN_POINT('',(-1.7442,-0.255,9.7));
#23410=CARTESIAN_POINT('',(-1.74047515456274,-0.167429513866972,9.6));
#23411=CARTESIAN_POINT('Ctrl Pts',(-1.74415870087061,-0.266244406628447,
9.70002284206962));
#23412=CARTESIAN_POINT('Ctrl Pts',(-1.74420569602547,-0.265459972719924,
9.76628025589696));
#23413=CARTESIAN_POINT('Ctrl Pts',(-1.73938151386138,-0.264675538811401,
9.83253088537814));
#23414=CARTESIAN_POINT('Ctrl Pts',(-1.72962299494269,-0.263891104902878,
9.89804654821063));
#23415=CARTESIAN_POINT('Ctrl Pts',(-1.69868589188987,-0.261404240567386,
10.1057486420951));
#23416=CARTESIAN_POINT('Ctrl Pts',(-1.61815580299121,-0.258917376231894,
10.306063888989));
#23417=CARTESIAN_POINT('Ctrl Pts',(-1.49671968419857,-0.256430511896403,
10.4773838643973));
#23418=CARTESIAN_POINT('Ctrl Pts',(-1.37528356540594,-0.253943647560911,
10.6487038398057));
#23419=CARTESIAN_POINT('Ctrl Pts',(-1.21294141671933,-0.25145678322542,
10.7910285437285));
#23420=CARTESIAN_POINT('Ctrl Pts',(-1.02720542034702,-0.248969918889928,
10.8890050939007));
#23421=CARTESIAN_POINT('Ctrl Pts',(-0.841469423974722,-0.246483054554436,
10.9869816440729));
#23422=CARTESIAN_POINT('Ctrl Pts',(-0.632339579916726,-0.243996190218945,
11.0406100404945));
#23423=CARTESIAN_POINT('Ctrl Pts',(-0.422375189109452,-0.241509325883453,
11.0441053064551));
#23424=CARTESIAN_POINT('Ctrl Pts',(-0.212410798302177,-0.239022461547962,
11.0476005724156));
#23425=CARTESIAN_POINT('Ctrl Pts',(-0.00161186074562417,-0.23653559721247,
11.000962707915));
#23426=CARTESIAN_POINT('Ctrl Pts',(0.187282340796658,-0.234048732876978,
10.9092225683747));
#23427=CARTESIAN_POINT('Ctrl Pts',(0.37617654233894,-0.231561868541487,
10.8174824288345));
#23428=CARTESIAN_POINT('Ctrl Pts',(0.543166007866952,-0.229075004205995,
10.6806400142546));
#23429=CARTESIAN_POINT('Ctrl Pts',(0.670237130981439,-0.226588139870503,
10.5134569577609));
#23430=CARTESIAN_POINT('Ctrl Pts',(0.797308254095925,-0.224101275535012,
10.3462739012672));
#23431=CARTESIAN_POINT('Ctrl Pts',(0.884461034796888,-0.22161441119952,
10.1487502028598));
#23432=CARTESIAN_POINT('Ctrl Pts',(0.9222943334795,-0.219127546864029,9.94219283449699));
#23433=CARTESIAN_POINT('Ctrl Pts',(0.960127632162113,-0.216640682528537,
9.73563546613418));
#23434=CARTESIAN_POINT('Ctrl Pts',(0.948641448826376,-0.214153818193045,
9.52004442781599));
#23435=CARTESIAN_POINT('Ctrl Pts',(0.889074364684035,-0.211666953857554,
9.31867669316543));
#23436=CARTESIAN_POINT('Ctrl Pts',(0.829507280541693,-0.209180089522062,
9.11730895851487));
#23437=CARTESIAN_POINT('Ctrl Pts',(0.721859295592745,-0.206693225186571,
8.93016452753194));
#23438=CARTESIAN_POINT('Ctrl Pts',(0.577743655398177,-0.204206360851079,
8.77742952694693));
#23439=CARTESIAN_POINT('Ctrl Pts',(0.43362801520361,-0.201719496515587,
8.62469452636193));
#23440=CARTESIAN_POINT('Ctrl Pts',(0.253044719763425,-0.199232632180096,
8.50636895617486));
#23441=CARTESIAN_POINT('Ctrl Pts',(0.0554715964079175,-0.196745767844604,
8.43522018029139));
#23442=CARTESIAN_POINT('Ctrl Pts',(-0.142101526947592,-0.194258903509113,
8.36407140440791));
#23443=CARTESIAN_POINT('Ctrl Pts',(-0.356664478218423,-0.191772039173621,
8.34009942282803));
#23444=CARTESIAN_POINT('Ctrl Pts',(-0.565066781035095,-0.189285174838129,
8.36588291802197));
#23445=CARTESIAN_POINT('Ctrl Pts',(-0.773469083851767,-0.186798310502638,
8.39166641321591));
#23446=CARTESIAN_POINT('Ctrl Pts',(-0.975710738214278,-0.184311446167146,
8.46720538518367));
#23447=CARTESIAN_POINT('Ctrl Pts',(-1.14998417762288,-0.181824581831655,
8.58436696040311));
#23448=CARTESIAN_POINT('Ctrl Pts',(-1.32425761703147,-0.179337717496163,
8.70152853562254));
#23449=CARTESIAN_POINT('Ctrl Pts',(-1.47056284148616,-0.176850853160671,
8.86031271409366));
#23450=CARTESIAN_POINT('Ctrl Pts',(-1.57308686213316,-0.17436398882518,
9.04355598262635));
#23451=CARTESIAN_POINT('Ctrl Pts',(-1.66838092966563,-0.172052497172444,
9.21387700882323));
#23452=CARTESIAN_POINT('Ctrl Pts',(-1.72585093496104,-0.169741005519708,
9.40532906990018));
#23453=CARTESIAN_POINT('Ctrl Pts',(-1.74046409013886,-0.167429513866973,
9.6000014831431));
#23454=CARTESIAN_POINT('',(-1.74047515456274,-0.153340700610567,9.6));
#23455=CARTESIAN_POINT('',(-1.74047515456274,-0.255,9.6));
#23456=CARTESIAN_POINT('Ctrl Pts',(-1.74047515456274,-0.153340700610567,
9.6));
#23457=CARTESIAN_POINT('Ctrl Pts',(-1.72473294771491,-0.155846150645574,
9.38897962842498));
#23458=CARTESIAN_POINT('Ctrl Pts',(-1.65828106796239,-0.158351600680581,
9.18182683781037));
#23459=CARTESIAN_POINT('Ctrl Pts',(-1.54831356305132,-0.160857050715588,
9.00111449525873));
#23460=CARTESIAN_POINT('Ctrl Pts',(-1.43834605814026,-0.163362500750596,
8.82040215270709));
#23461=CARTESIAN_POINT('Ctrl Pts',(-1.28486292807066,-0.165867950785603,
8.66613025821842));
#23462=CARTESIAN_POINT('Ctrl Pts',(-1.10470058034043,-0.16837340082061,
8.55522077011294));
#23463=CARTESIAN_POINT('Ctrl Pts',(-0.924538232610208,-0.170878850855617,
8.44431128200746));
#23464=CARTESIAN_POINT('Ctrl Pts',(-0.717696667219359,-0.173384300890624,
8.37676420028517));
#23465=CARTESIAN_POINT('Ctrl Pts',(-0.506806067411535,-0.175889750925631,
8.3599572690053));
#23466=CARTESIAN_POINT('Ctrl Pts',(-0.295915467603711,-0.178395200960638,
8.34315033772542));
#23467=CARTESIAN_POINT('Ctrl Pts',(-0.0809758333789124,-0.180900650995646,
8.37708355688795));
#23468=CARTESIAN_POINT('Ctrl Pts',(0.114479473573055,-0.183406101030653,
8.45804996515167));
#23469=CARTESIAN_POINT('Ctrl Pts',(0.309934780525024,-0.18591155106566,
8.53901637341539));
#23470=CARTESIAN_POINT('Ctrl Pts',(0.485905760204162,-0.188417001100667,
8.66701597078031));
#23471=CARTESIAN_POINT('Ctrl Pts',(0.6231331327789,-0.190922451135674,8.82803444612455));
#23472=CARTESIAN_POINT('Ctrl Pts',(0.760360505353638,-0.193427901170681,
8.9890529214688));
#23473=CARTESIAN_POINT('Ctrl Pts',(0.858844270823975,-0.195933351205688,
9.18309027479239));
#23474=CARTESIAN_POINT('Ctrl Pts',(0.907803125803339,-0.198438801240696,
9.38890870639347));
#23475=CARTESIAN_POINT('Ctrl Pts',(0.956761980782702,-0.200944251275703,
9.59472713799455));
#23476=CARTESIAN_POINT('Ctrl Pts',(0.956195925271092,-0.20344970131071,
9.81232664787314));
#23477=CARTESIAN_POINT('Ctrl Pts',(0.90616748485386,-0.205955151345717,
10.0178879803874));
#23478=CARTESIAN_POINT('Ctrl Pts',(0.856139044436628,-0.208460601380724,
10.2234493129017));
#23479=CARTESIAN_POINT('Ctrl Pts',(0.756648219113773,-0.210966051415731,
10.4169724680517));
#23480=CARTESIAN_POINT('Ctrl Pts',(0.618585043209539,-0.213471501450739,
10.5772746807812));
#23481=CARTESIAN_POINT('Ctrl Pts',(0.480521867305305,-0.215976951485746,
10.7375768935107));
#23482=CARTESIAN_POINT('Ctrl Pts',(0.303886340819692,-0.218482401520753,
10.8646581638196));
#23483=CARTESIAN_POINT('Ctrl Pts',(0.108013169915432,-0.22098785155576,
10.9446079735783));
#23484=CARTESIAN_POINT('Ctrl Pts',(-0.0878600009888281,-0.223493301590767,
11.0245577833369));
#23485=CARTESIAN_POINT('Ctrl Pts',(-0.302970816311735,-0.225998751625774,
11.0573761325454));
#23486=CARTESIAN_POINT('Ctrl Pts',(-0.513773231433628,-0.228504201660781,
11.0394707880266));
#23487=CARTESIAN_POINT('Ctrl Pts',(-0.724575646555521,-0.231009651695789,
11.0215654435079));
#23488=CARTESIAN_POINT('Ctrl Pts',(-0.9310696614764,-0.233515101730796,
10.9529364052621));
#23489=CARTESIAN_POINT('Ctrl Pts',(-1.1106523459517,-0.236020551765803,
10.8410957962038));
#23490=CARTESIAN_POINT('Ctrl Pts',(-1.290235030427,-0.23852600180081,10.7292551871455));
#23491=CARTESIAN_POINT('Ctrl Pts',(-1.44290638445672,-0.241031451835817,
10.5742030072748));
#23492=CARTESIAN_POINT('Ctrl Pts',(-1.55195496298315,-0.243536901870824,
10.3929113359787));
#23493=CARTESIAN_POINT('Ctrl Pts',(-1.66100354150958,-0.246042351905831,
10.2116196646827));
#23494=CARTESIAN_POINT('Ctrl Pts',(-1.72642934453273,-0.248547801940839,
10.0040885019612));
#23495=CARTESIAN_POINT('Ctrl Pts',(-1.74107083610881,-0.251053251975846,
9.79303427067891));
#23496=CARTESIAN_POINT('Ctrl Pts',(-1.74321814458179,-0.251420699107911,
9.76208123992141));
#23497=CARTESIAN_POINT('Ctrl Pts',(-1.74427313829983,-0.251788146239977,
9.73105243182909));
#23498=CARTESIAN_POINT('Ctrl Pts',(-1.74424829702886,-0.252155593372042,
9.70002193782831));
#23499=CARTESIAN_POINT('Origin',(-0.4,-0.255,9.7));
#23500=CARTESIAN_POINT('',(-1.74415902867232,-0.366244406628447,9.69997584025059));
#23501=CARTESIAN_POINT('',(-1.74411350535466,-0.352155593372042,9.70000771515446));
#23502=CARTESIAN_POINT('',(-1.7442,-0.255,9.7));
#23503=CARTESIAN_POINT('Ctrl Pts',(-1.74415902867232,-0.366244406628447,
9.69997584025059));
#23504=CARTESIAN_POINT('Ctrl Pts',(-1.74404578241023,-0.364455875747981,
9.85103608154908));
#23505=CARTESIAN_POINT('Ctrl Pts',(-1.7185672270758,-0.362667344867516,
10.0021470613059));
#23506=CARTESIAN_POINT('Ctrl Pts',(-1.66861307355174,-0.36087881398705,
10.1446731556306));
#23507=CARTESIAN_POINT('Ctrl Pts',(-1.59915427685692,-0.358391949651559,
10.342848688815));
#23508=CARTESIAN_POINT('Ctrl Pts',(-1.48237549311787,-0.355905085316067,
10.5244266024324));
#23509=CARTESIAN_POINT('Ctrl Pts',(-1.3308763368522,-0.353418220980575,
10.6698374482951));
#23510=CARTESIAN_POINT('Ctrl Pts',(-1.17937718058652,-0.350931356645084,
10.8152482941577));
#23511=CARTESIAN_POINT('Ctrl Pts',(-0.993157651794214,-0.348444492309592,
10.9244920722656));
#23512=CARTESIAN_POINT('Ctrl Pts',(-0.792305418029019,-0.345957627974101,
10.9857755739092));
#23513=CARTESIAN_POINT('Ctrl Pts',(-0.591453184263824,-0.343470763638609,
11.0470590755528));
#23514=CARTESIAN_POINT('Ctrl Pts',(-0.375968245525741,-0.340983899303117,
11.0603823007321));
#23515=CARTESIAN_POINT('Ctrl Pts',(-0.169095752144418,-0.338497034967626,
11.0243119578645));
#23516=CARTESIAN_POINT('Ctrl Pts',(0.0377767412369071,-0.336010170632134,
10.988241614997));
#23517=CARTESIAN_POINT('Ctrl Pts',(0.236036789261473,-0.333523306296643,
10.9027777040825));
#23518=CARTESIAN_POINT('Ctrl Pts',(0.40429775759656,-0.331036441961151,
10.7771375488516));
#23519=CARTESIAN_POINT('Ctrl Pts',(0.572558725931644,-0.328549577625659,
10.6514973936206));
#23520=CARTESIAN_POINT('Ctrl Pts',(0.71082061457725,-0.326062713290168,
10.4856809940731));
#23521=CARTESIAN_POINT('Ctrl Pts',(0.80416876135257,-0.323575848954676,
10.2975761605154));
#23522=CARTESIAN_POINT('Ctrl Pts',(0.897516908127891,-0.321088984619184,
10.1094713269576));
#23523=CARTESIAN_POINT('Ctrl Pts',(0.945951313032926,-0.318602120283693,
9.8990780593896));
#23524=CARTESIAN_POINT('Ctrl Pts',(0.944247277856241,-0.316115255948201,
9.68909153369745));
#23525=CARTESIAN_POINT('Ctrl Pts',(0.942543242679555,-0.31362839161271,
9.4791050080053));
#23526=CARTESIAN_POINT('Ctrl Pts',(0.890700767421149,-0.311141527277218,
9.26952522418903));
#23527=CARTESIAN_POINT('Ctrl Pts',(0.794312198032813,-0.308654662941726,
9.08296017850674));
#23528=CARTESIAN_POINT('Ctrl Pts',(0.69792362864448,-0.306167798606235,
8.89639513282446));
#23529=CARTESIAN_POINT('Ctrl Pts',(0.556988965126219,-0.303680934270743,
8.73284482527617));
#23530=CARTESIAN_POINT('Ctrl Pts',(0.3867111337889,-0.301194069935252,8.60995169102424));
#23531=CARTESIAN_POINT('Ctrl Pts',(0.216433302451579,-0.29870720559976,
8.48705855677231));
#23532=CARTESIAN_POINT('Ctrl Pts',(0.0168123032952003,-0.296220341264268,
8.40482259581673));
#23533=CARTESIAN_POINT('Ctrl Pts',(-0.190618325459444,-0.293733476928777,
8.37211481407425));
#23534=CARTESIAN_POINT('Ctrl Pts',(-0.398048954214088,-0.291246612593285,
8.33940703233177));
#23535=CARTESIAN_POINT('Ctrl Pts',(-0.613289212566997,-0.288759748257794,
8.35622742980239));
#23536=CARTESIAN_POINT('Ctrl Pts',(-0.813120676364068,-0.286272883922302,
8.42076153704854));
#23537=CARTESIAN_POINT('Ctrl Pts',(-1.01295214016114,-0.28378601958681,
8.48529564429469));
#23538=CARTESIAN_POINT('Ctrl Pts',(-1.19737480940237,-0.281299155251319,
8.59754346131637));
#23539=CARTESIAN_POINT('Ctrl Pts',(-1.34649461965064,-0.278812290915827,
8.7453965855336));
#23540=CARTESIAN_POINT('Ctrl Pts',(-1.4956144298989,-0.276325426580336,
8.89324970975083));
#23541=CARTESIAN_POINT('Ctrl Pts',(-1.6094313811542,-0.273838562244844,
9.0767081411636));
#23542=CARTESIAN_POINT('Ctrl Pts',(-1.67566779817835,-0.271351697909352,
9.27598182730744));
#23543=CARTESIAN_POINT('Ctrl Pts',(-1.72101120115614,-0.269649267482384,
9.41239843103761));
#23544=CARTESIAN_POINT('Ctrl Pts',(-1.74405670887271,-0.267946837055416,
9.55622661387719));
#23545=CARTESIAN_POINT('Ctrl Pts',(-1.74415870087061,-0.266244406628447,
9.70002284206962));
#23546=CARTESIAN_POINT('Ctrl Pts',(-1.74424829702886,-0.252155593372042,
9.70002193782831));
#23547=CARTESIAN_POINT('Ctrl Pts',(-1.74410375729837,-0.254293596274984,
9.51947001494231));
#23548=CARTESIAN_POINT('Ctrl Pts',(-1.70740106403156,-0.256431599177926,
9.33886101509463));
#23549=CARTESIAN_POINT('Ctrl Pts',(-1.63659858427149,-0.258569602080867,
9.17279007747477));
#23550=CARTESIAN_POINT('Ctrl Pts',(-1.55362766072905,-0.261075052115874,
8.97817741539611));
#23551=CARTESIAN_POINT('Ctrl Pts',(-1.42382863351516,-0.263580502150882,
8.80352939108198));
#23552=CARTESIAN_POINT('Ctrl Pts',(-1.26140934623515,-0.266085952185889,
8.6679630339014));
#23553=CARTESIAN_POINT('Ctrl Pts',(-1.09899005895515,-0.268591402220896,
8.53239667672083));
#23554=CARTESIAN_POINT('Ctrl Pts',(-0.903950511609032,-0.271096852255903,
8.43591198667381));
#23555=CARTESIAN_POINT('Ctrl Pts',(-0.697639798691326,-0.27360230229091,
8.38907021096974));
#23556=CARTESIAN_POINT('Ctrl Pts',(-0.49132908577362,-0.276107752325917,
8.34222843526567));
#23557=CARTESIAN_POINT('Ctrl Pts',(-0.273747207284324,-0.278613202360924,
8.34502957390454));
#23558=CARTESIAN_POINT('Ctrl Pts',(-0.0687107480140969,-0.281118652395932,
8.39716701276829));
#23559=CARTESIAN_POINT('Ctrl Pts',(0.136325711256132,-0.283624102430939,
8.44930445163204));
#23560=CARTESIAN_POINT('Ctrl Pts',(0.328816751307292,-0.286129552465946,
8.55077819072068));
#23561=CARTESIAN_POINT('Ctrl Pts',(0.487692238606602,-0.288635002500953,
8.69048088128578));
#23562=CARTESIAN_POINT('Ctrl Pts',(0.646567725905912,-0.29114045253596,
8.83018357185089));
#23563=CARTESIAN_POINT('Ctrl Pts',(0.771827660453372,-0.293645902570967,
9.00811521389247));
#23564=CARTESIAN_POINT('Ctrl Pts',(0.849761047925756,-0.296151352605974,
9.20479934949277));
#23565=CARTESIAN_POINT('Ctrl Pts',(0.927694435398139,-0.298656802640981,
9.40148348509306));
#23566=CARTESIAN_POINT('Ctrl Pts',(0.958301275795446,-0.301162252675989,
9.61692011425207));
#23567=CARTESIAN_POINT('Ctrl Pts',(0.938231334443277,-0.303667702710996,
9.82752747368889));
#23568=CARTESIAN_POINT('Ctrl Pts',(0.918161393091109,-0.306173152746003,
10.0381348331257));
#23569=CARTESIAN_POINT('Ctrl Pts',(0.847414669989466,-0.30867860278101,
10.2439129228403));
#23570=CARTESIAN_POINT('Ctrl Pts',(0.733735124390046,-0.311184052816017,
10.4223372001404));
#23571=CARTESIAN_POINT('Ctrl Pts',(0.620055578790627,-0.313689502851024,
10.6007614774404));
#23572=CARTESIAN_POINT('Ctrl Pts',(0.463443210693432,-0.316194952886031,
10.7518319423259));
#23573=CARTESIAN_POINT('Ctrl Pts',(0.281040863626771,-0.318700402921038,
10.8590123805809));
#23574=CARTESIAN_POINT('Ctrl Pts',(0.0986385165601081,-0.321205852956046,
10.9661928188359));
#23575=CARTESIAN_POINT('Ctrl Pts',(-0.10955380947602,-0.323711302991053,
11.0294832304604));
#23576=CARTESIAN_POINT('Ctrl Pts',(-0.320747316145784,-0.32621675302606,
11.0419558059126));
#23577=CARTESIAN_POINT('Ctrl Pts',(-0.531940822815548,-0.328722203061067,
11.0544283813648));
#23578=CARTESIAN_POINT('Ctrl Pts',(-0.746135510118948,-0.331227653096074,
11.0160831206447));
#23579=CARTESIAN_POINT('Ctrl Pts',(-0.939885549343526,-0.333733103131081,
10.9311173517491));
#23580=CARTESIAN_POINT('Ctrl Pts',(-1.1336355885681,-0.336238553166089,
10.8461515828534));
#23581=CARTESIAN_POINT('Ctrl Pts',(-1.30694097971386,-0.338744003201096,
10.7145653057822));
#23582=CARTESIAN_POINT('Ctrl Pts',(-1.44083167143585,-0.341249453236103,
10.5507619058457));
#23583=CARTESIAN_POINT('Ctrl Pts',(-1.57472236315784,-0.34375490327111,
10.3869585059092));
#23584=CARTESIAN_POINT('Ctrl Pts',(-1.66919835545607,-0.346260353306117,
10.1909379831076));
#23585=CARTESIAN_POINT('Ctrl Pts',(-1.71391824344407,-0.348765803341124,
9.98415700824511));
#23586=CARTESIAN_POINT('Ctrl Pts',(-1.73408641394803,-0.34989573335143,
9.89090109581708));
#23587=CARTESIAN_POINT('Ctrl Pts',(-1.7441346438382,-0.351025663361736,
9.79545660497557));
#23588=CARTESIAN_POINT('Ctrl Pts',(-1.74411350535466,-0.352155593372042,
9.70000771515446));
#23589=CARTESIAN_POINT('Origin',(-0.4,0.0506589891902575,9.7));
#23590=CARTESIAN_POINT('',(-1.68683546212087,-0.299341010809742,9.70002186794253));
#23591=CARTESIAN_POINT('',(-1.68679219402118,-0.319058989190747,9.70000738613257));
#23592=CARTESIAN_POINT('',(-1.686875,0.0506589891902575,9.7));
#23593=CARTESIAN_POINT('',(-0.517805766168008,-0.3758,10.9813944679847));
#23594=CARTESIAN_POINT('Ctrl Pts',(-1.68683546212087,-0.299341010809742,
9.70002186794253));
#23595=CARTESIAN_POINT('Ctrl Pts',(-1.68673781969243,-0.301043441236711,
9.56235800009911));
#23596=CARTESIAN_POINT('Ctrl Pts',(-1.63244651236718,-0.305232735999171,
9.22352319669137));
#23597=CARTESIAN_POINT('Ctrl Pts',(-1.33992756310779,-0.311908895097122,
8.75201990128797));
#23598=CARTESIAN_POINT('Ctrl Pts',(-0.810254324423489,-0.319369488103597,
8.42963727326435));
#23599=CARTESIAN_POINT('Ctrl Pts',(-0.192071076094596,-0.326830081110072,
8.38132805812896));
#23600=CARTESIAN_POINT('Ctrl Pts',(0.381252700031053,-0.334290674116547,
8.61751479132649));
#23601=CARTESIAN_POINT('Ctrl Pts',(0.786025713976292,-0.341751267123022,
9.08724132463895));
#23602=CARTESIAN_POINT('Ctrl Pts',(0.934920488596498,-0.349211860129497,
9.68916734226706));
#23603=CARTESIAN_POINT('Ctrl Pts',(0.795813901454333,-0.356672453135971,
10.2934297352181));
#23604=CARTESIAN_POINT('Ctrl Pts',(0.398717261183206,-0.364133046142446,
10.7696646240018));
#23605=CARTESIAN_POINT('Ctrl Pts',(-0.0879068301996579,-0.370508895097122,
10.9794335532901));
#23606=CARTESIAN_POINT('Ctrl Pts',(-0.404889468122248,-0.374397879716307,
10.9917424685781));
#23607=CARTESIAN_POINT('Ctrl Pts',(-0.517805766168008,-0.3758,10.9813944679847));
#23608=CARTESIAN_POINT('',(0.773161008253381,-0.3758,10.228905014477));
#23609=CARTESIAN_POINT('Origin',(-0.4,-0.3758,9.7));
#23610=CARTESIAN_POINT('Ctrl Pts',(-1.68679219402118,-0.319058989190747,
9.70000738613257));
#23611=CARTESIAN_POINT('Ctrl Pts',(-1.68676755850452,-0.320434509215448,
9.58876796298132));
#23612=CARTESIAN_POINT('Ctrl Pts',(-1.64639120365236,-0.324315479275156,
9.27489314898718));
#23613=CARTESIAN_POINT('Ctrl Pts',(-1.39395194797187,-0.330701899369872,
8.80772380021452));
#23614=CARTESIAN_POINT('Ctrl Pts',(-0.879252204171272,-0.338218249474893,
8.45324089690315));
#23615=CARTESIAN_POINT('Ctrl Pts',(-0.259635570614986,-0.345734599579915,
8.3716914957747));
#23616=CARTESIAN_POINT('Ctrl Pts',(0.329254578046856,-0.353250949684936,
8.58095279849071));
#23617=CARTESIAN_POINT('Ctrl Pts',(0.758488001187141,-0.360767299789957,
9.03515948120896));
#23618=CARTESIAN_POINT('Ctrl Pts',(0.934107096026125,-0.368283649894978,
9.63498649925687));
#23619=CARTESIAN_POINT('Ctrl Pts',(0.856422329660891,-0.373294549964993,
10.0442235818997));
#23620=CARTESIAN_POINT('Ctrl Pts',(0.773161008253379,-0.3758,10.228905014477));
#23621=CARTESIAN_POINT('Origin',(-0.4,0.0506589891902575,9.7));
#23622=CARTESIAN_POINT('',(-1.686875,-0.2,9.7));
#23623=CARTESIAN_POINT('',(-1.6869212373449,-0.219058989190747,9.70002100226366));
#23624=CARTESIAN_POINT('',(-1.686875,0.0506589891902575,9.7));
#23625=CARTESIAN_POINT('',(-1.68577203777491,-0.2,9.64673150554831));
#23626=CARTESIAN_POINT('Origin',(-0.4,-0.2,9.7));
#23627=CARTESIAN_POINT('Ctrl Pts',(-1.68577203777491,-0.2,9.64673150554831));
#23628=CARTESIAN_POINT('Ctrl Pts',(-1.67744860675331,-0.202486864335492,
9.44582410285027));
#23629=CARTESIAN_POINT('Ctrl Pts',(-1.56497328697934,-0.207460593006475,
9.04813481150073));
#23630=CARTESIAN_POINT('Ctrl Pts',(-1.14477569200808,-0.21492118601295,
8.59209689377269));
#23631=CARTESIAN_POINT('Ctrl Pts',(-0.563925233093278,-0.222381779019424,
8.3751443244727));
#23632=CARTESIAN_POINT('Ctrl Pts',(0.0523127476759186,-0.229842372025899,
8.44399332862896));
#23633=CARTESIAN_POINT('Ctrl Pts',(0.570959068877206,-0.237302965032374,
8.78383163721656));
#23634=CARTESIAN_POINT('Ctrl Pts',(0.880130696531965,-0.244763558038849,
9.32132194287307));
#23635=CARTESIAN_POINT('Ctrl Pts',(0.913119720888853,-0.252224151045324,
9.94051265281741));
#23636=CARTESIAN_POINT('Ctrl Pts',(0.662811579247987,-0.259684744051799,
10.5078128523146));
#23637=CARTESIAN_POINT('Ctrl Pts',(0.183207572884291,-0.267145337058273,
10.9008326758436));
#23638=CARTESIAN_POINT('Ctrl Pts',(-0.422219929201908,-0.274605930064748,
11.0347794885482));
#23639=CARTESIAN_POINT('Ctrl Pts',(-1.02285369219581,-0.282066523071223,
10.8807554386038));
#23640=CARTESIAN_POINT('Ctrl Pts',(-1.48911031901715,-0.289527116077698,
10.4719901431999));
#23641=CARTESIAN_POINT('Ctrl Pts',(-1.6676202903207,-0.295285278657204,
10.0279540138011));
#23642=CARTESIAN_POINT('Ctrl Pts',(-1.68688045311172,-0.298556576901219,
9.76345365593468));
#23643=CARTESIAN_POINT('Ctrl Pts',(-1.68683546212087,-0.299341010809742,
9.70002186794253));
#23644=CARTESIAN_POINT('Ctrl Pts',(-1.6869212373449,-0.219058989190747,
9.70002100226366));
#23645=CARTESIAN_POINT('Ctrl Pts',(-1.68678286168229,-0.221196992093688,
9.52716892983104));
#23646=CARTESIAN_POINT('Ctrl Pts',(-1.61046904669073,-0.225840445031637,
9.15163894624125));
#23647=CARTESIAN_POINT('Ctrl Pts',(-1.25590265556386,-0.232989348004593,
8.67456048866193));
#23648=CARTESIAN_POINT('Ctrl Pts',(-0.695737090563785,-0.240505698109614,
8.39745052994095));
#23649=CARTESIAN_POINT('Ctrl Pts',(-0.0708285653125278,-0.248022048214636,
8.40549557223947));
#23650=CARTESIAN_POINT('Ctrl Pts',(0.482017530132723,-0.255538398319657,
8.69693438638102));
#23651=CARTESIAN_POINT('Ctrl Pts',(0.841771759274435,-0.263054748424679,
9.20796499607955));
#23652=CARTESIAN_POINT('Ctrl Pts',(0.929676485661023,-0.2705710985297,9.8267122334304));
#23653=CARTESIAN_POINT('Ctrl Pts',(0.726487549584337,-0.278087448634722,
10.4177195519875));
#23654=CARTESIAN_POINT('Ctrl Pts',(0.276687204706167,-0.285603798739743,
10.8516032102962));
#23655=CARTESIAN_POINT('Ctrl Pts',(-0.321253948919206,-0.293120148844764,
11.0333771616263));
#23656=CARTESIAN_POINT('Ctrl Pts',(-0.936434252944416,-0.300636498949786,
10.923247216553));
#23657=CARTESIAN_POINT('Ctrl Pts',(-1.43417798579078,-0.308152849054807,
10.5453233429344));
#23658=CARTESIAN_POINT('Ctrl Pts',(-1.65586245541949,-0.314293679135128,
10.0853683366248));
#23659=CARTESIAN_POINT('Ctrl Pts',(-1.68681243102907,-0.317929059180441,
9.7913857450736));
#23660=CARTESIAN_POINT('Ctrl Pts',(-1.68679219402118,-0.319058989190747,
9.70000738613257));
#23661=CARTESIAN_POINT('Ctrl Pts',(-1.68330900500515,-0.120244096429272,
9.60426461836037));
#23662=CARTESIAN_POINT('Ctrl Pts',(-1.66823814320088,-0.122749546464279,
9.40224346029563));
#23663=CARTESIAN_POINT('Ctrl Pts',(-1.5410022218253,-0.127760446534293,
9.00560643095153));
#23664=CARTESIAN_POINT('Ctrl Pts',(-1.10018924085152,-0.135276796639315,
8.56252807009725));
#23665=CARTESIAN_POINT('Ctrl Pts',(-0.506127554802531,-0.142793146744336,
8.36852870067744));
#23666=CARTESIAN_POINT('Ctrl Pts',(0.111192282557321,-0.150309496849357,
8.46598699128103));
#23667=CARTESIAN_POINT('Ctrl Pts',(0.616591749469812,-0.157825846954379,
8.83360970038453));
#23668=CARTESIAN_POINT('Ctrl Pts',(0.899443175648149,-0.1653421970594,9.39089690256787));
#23669=CARTESIAN_POINT('Ctrl Pts',(0.897817429435154,-0.172858547164422,
10.0158560662526));
#23670=CARTESIAN_POINT('Ctrl Pts',(0.612073665477375,-0.180374897269443,
10.5716664596844));
#23671=CARTESIAN_POINT('Ctrl Pts',(0.104765579300823,-0.187891247374464,
10.9366516770526));
#23672=CARTESIAN_POINT('Ctrl Pts',(-0.513045900691733,-0.195407597479486,
11.0309079926402));
#23673=CARTESIAN_POINT('Ctrl Pts',(-1.10610940043427,-0.202923947584507,
10.8338011775994));
#23674=CARTESIAN_POINT('Ctrl Pts',(-1.54459091073853,-0.210440297689529,
10.3884817891799));
#23675=CARTESIAN_POINT('Ctrl Pts',(-1.73249783738354,-0.21795664779455,
9.79243953722229));
#23676=CARTESIAN_POINT('Ctrl Pts',(-1.62869343776713,-0.225472997899572,
9.1761603464716));
#23677=CARTESIAN_POINT('Ctrl Pts',(-1.25590265556386,-0.232989348004593,
8.67456048866193));
#23678=CARTESIAN_POINT('Ctrl Pts',(-0.695737090563785,-0.240505698109614,
8.39745052994095));
#23679=CARTESIAN_POINT('Ctrl Pts',(-0.0708285653125278,-0.248022048214636,
8.40549557223947));
#23680=CARTESIAN_POINT('Ctrl Pts',(0.482017530132723,-0.255538398319657,
8.69693438638102));
#23681=CARTESIAN_POINT('Ctrl Pts',(0.841771759274435,-0.263054748424679,
9.20796499607955));
#23682=CARTESIAN_POINT('Ctrl Pts',(0.929676485661023,-0.2705710985297,9.8267122334304));
#23683=CARTESIAN_POINT('Ctrl Pts',(0.726487549584337,-0.278087448634722,
10.4177195519875));
#23684=CARTESIAN_POINT('Ctrl Pts',(0.276687204706167,-0.285603798739743,
10.8516032102962));
#23685=CARTESIAN_POINT('Ctrl Pts',(-0.321253948919206,-0.293120148844764,
11.0333771616263));
#23686=CARTESIAN_POINT('Ctrl Pts',(-0.936434252944416,-0.300636498949786,
10.923247216553));
#23687=CARTESIAN_POINT('Ctrl Pts',(-1.43417798579078,-0.308152849054807,
10.5453233429344));
#23688=CARTESIAN_POINT('Ctrl Pts',(-1.7055188411444,-0.315669199159829,
9.98234035614576));
#23689=CARTESIAN_POINT('Ctrl Pts',(-1.69105451839558,-0.32318554926485,
9.35754801027796));
#23690=CARTESIAN_POINT('Ctrl Pts',(-1.39395194797187,-0.330701899369872,
8.80772380021452));
#23691=CARTESIAN_POINT('Ctrl Pts',(-0.879252204171272,-0.338218249474893,
8.45324089690315));
#23692=CARTESIAN_POINT('Ctrl Pts',(-0.259635570614986,-0.345734599579915,
8.3716914957747));
#23693=CARTESIAN_POINT('Ctrl Pts',(0.329254578046856,-0.353250949684936,
8.58095279849071));
#23694=CARTESIAN_POINT('Ctrl Pts',(0.758488001187141,-0.360767299789957,
9.03515948120896));
#23695=CARTESIAN_POINT('Ctrl Pts',(0.934107096026125,-0.368283649894978,
9.63498649925687));
#23696=CARTESIAN_POINT('Ctrl Pts',(0.856422329660891,-0.373294549964993,
10.0442235818997));
#23697=CARTESIAN_POINT('Ctrl Pts',(0.773161008253379,-0.3758,10.228905014477));
#23698=CARTESIAN_POINT('Ctrl Pts',(-1.70236438819101,-0.131276297823037,
9.60284307890691));
#23699=CARTESIAN_POINT('Ctrl Pts',(-1.68706974470556,-0.133781747858044,
9.39782218300541));
#23700=CARTESIAN_POINT('Ctrl Pts',(-1.55794454395348,-0.138792647928058,
8.99529563636627));
#23701=CARTESIAN_POINT('Ctrl Pts',(-1.1105860932347,-0.14630899803308,8.54563816797476));
#23702=CARTESIAN_POINT('Ctrl Pts',(-0.50770340381119,-0.153825348138101,
8.34875817330592));
#23703=CARTESIAN_POINT('Ctrl Pts',(0.118782788653509,-0.161341698243123,
8.44766358620418));
#23704=CARTESIAN_POINT('Ctrl Pts',(0.631686746274308,-0.168858048348144,
8.82074498963809));
#23705=CARTESIAN_POINT('Ctrl Pts',(0.918738129196869,-0.176374398453165,
9.38630714441723));
#23706=CARTESIAN_POINT('Ctrl Pts',(0.917088242876597,-0.183890748558187,
10.0205460967523));
#23707=CARTESIAN_POINT('Ctrl Pts',(0.627101574915222,-0.191407098663208,
10.5846095141902));
#23708=CARTESIAN_POINT('Ctrl Pts',(0.112260657645241,-0.19892344876823,
10.9550142627446));
#23709=CARTESIAN_POINT('Ctrl Pts',(-0.514724477672702,-0.206439798873251,
11.050670155678));
#23710=CARTESIAN_POINT('Ctrl Pts',(-1.11659415908861,-0.213956148978272,
10.8506365740717));
#23711=CARTESIAN_POINT('Ctrl Pts',(-1.56158651998784,-0.221472499083294,
10.3987048019213));
#23712=CARTESIAN_POINT('Ctrl Pts',(-1.75228360744098,-0.228988849188315,
9.79381213789479));
#23713=CARTESIAN_POINT('Ctrl Pts',(-1.6469378544924,-0.236505199293337,
9.16838204421781));
#23714=CARTESIAN_POINT('Ctrl Pts',(-1.26861163914299,-0.244021549398358,
8.65933411469724));
#23715=CARTESIAN_POINT('Ctrl Pts',(-0.700128381796828,-0.25153789950338,
8.37810945216957));
#23716=CARTESIAN_POINT('Ctrl Pts',(-0.0659408198066945,-0.259054249608401,
8.38627395234078));
#23717=CARTESIAN_POINT('Ctrl Pts',(0.495114283874633,-0.266570599713422,
8.68204023419045));
#23718=CARTESIAN_POINT('Ctrl Pts',(0.860210371183234,-0.274086949818444,
9.20065894936438));
#23719=CARTESIAN_POINT('Ctrl Pts',(0.949420362504933,-0.281603299923465,
9.82859373675729));
#23720=CARTESIAN_POINT('Ctrl Pts',(0.743214348685499,-0.289119650028487,
10.42837670551));
#23721=CARTESIAN_POINT('Ctrl Pts',(0.286735084002856,-0.296636000133508,
10.8687029426013));
#23722=CARTESIAN_POINT('Ctrl Pts',(-0.320084677783521,-0.304152350238529,
11.0531759884458));
#23723=CARTESIAN_POINT('Ctrl Pts',(-0.944399567770392,-0.311668700343551,
10.9414107643435));
#23724=CARTESIAN_POINT('Ctrl Pts',(-1.44953411414706,-0.319185050448572,
10.5578752381932));
#23725=CARTESIAN_POINT('Ctrl Pts',(-1.72490401001437,-0.326701400553594,
9.98653272419914));
#23726=CARTESIAN_POINT('Ctrl Pts',(-1.7102249118596,-0.334217750658615,
9.35246306669736));
#23727=CARTESIAN_POINT('Ctrl Pts',(-1.40871077469487,-0.341734100763636,
8.79447471926191));
#23728=CARTESIAN_POINT('Ctrl Pts',(-0.886368443796752,-0.349250450868658,
8.43472822976116));
#23729=CARTESIAN_POINT('Ctrl Pts',(-0.257551350854068,-0.35676680097368,
8.35196793158375));
#23730=CARTESIAN_POINT('Ctrl Pts',(0.340083010926646,-0.364283151078701,
8.56433647838023));
#23731=CARTESIAN_POINT('Ctrl Pts',(0.775689963218691,-0.371799501183722,
9.02528750899211));
#23732=CARTESIAN_POINT('Ctrl Pts',(0.953916761372978,-0.379315851288744,
9.63402113770787));
#23733=CARTESIAN_POINT('Ctrl Pts',(0.875078482498271,-0.384326751358758,
10.0493348312006));
#23734=CARTESIAN_POINT('Ctrl Pts',(0.790580844367512,-0.386832201393765,
10.2367585304116));
#23735=CARTESIAN_POINT('Ctrl Pts',(-1.72141977137688,-0.142308499216802,
9.60142153945346));
#23736=CARTESIAN_POINT('Ctrl Pts',(-1.70590134621024,-0.144813949251809,
9.3934009057152));
#23737=CARTESIAN_POINT('Ctrl Pts',(-1.57488686608167,-0.149824849321823,
8.98498484178101));
#23738=CARTESIAN_POINT('Ctrl Pts',(-1.12098294561788,-0.157341199426845,
8.52874826585226));
#23739=CARTESIAN_POINT('Ctrl Pts',(-0.509279252819849,-0.164857549531866,
8.3289876459344));
#23740=CARTESIAN_POINT('Ctrl Pts',(0.126373294749698,-0.172373899636888,
8.42934018112733));
#23741=CARTESIAN_POINT('Ctrl Pts',(0.646781743078804,-0.179890249741909,
8.80788027889165));
#23742=CARTESIAN_POINT('Ctrl Pts',(0.93803308274559,-0.18740659984693,9.3817173862666));
#23743=CARTESIAN_POINT('Ctrl Pts',(0.93635905631804,-0.194922949951952,
10.025236127252));
#23744=CARTESIAN_POINT('Ctrl Pts',(0.64212948435307,-0.202439300056973,
10.597552568696));
#23745=CARTESIAN_POINT('Ctrl Pts',(0.119755735989659,-0.209955650161995,
10.9733768484366));
#23746=CARTESIAN_POINT('Ctrl Pts',(-0.516403054653671,-0.217472000267016,
11.0704323187159));
#23747=CARTESIAN_POINT('Ctrl Pts',(-1.12707891774294,-0.224988350372037,
10.867471970544));
#23748=CARTESIAN_POINT('Ctrl Pts',(-1.57858212923714,-0.232504700477059,
10.4089278146627));
#23749=CARTESIAN_POINT('Ctrl Pts',(-1.77206937749842,-0.24002105058208,
9.79518473856729));
#23750=CARTESIAN_POINT('Ctrl Pts',(-1.66518227121767,-0.247537400687102,
9.16060374196403));
#23751=CARTESIAN_POINT('Ctrl Pts',(-1.28132062272213,-0.255053750792123,
8.64410774073254));
#23752=CARTESIAN_POINT('Ctrl Pts',(-0.704519673029873,-0.262570100897145,
8.35876837439818));
#23753=CARTESIAN_POINT('Ctrl Pts',(-0.06105307430086,-0.270086451002166,
8.36705233244209));
#23754=CARTESIAN_POINT('Ctrl Pts',(0.508211037616542,-0.277602801107187,
8.66714608199988));
#23755=CARTESIAN_POINT('Ctrl Pts',(0.878648983092034,-0.285119151212209,
9.19335290264921));
#23756=CARTESIAN_POINT('Ctrl Pts',(0.969164239348842,-0.29263550131723,
9.83047524008419));
#23757=CARTESIAN_POINT('Ctrl Pts',(0.759941147786661,-0.300151851422252,
10.4390338590325));
#23758=CARTESIAN_POINT('Ctrl Pts',(0.296782963299545,-0.307668201527273,
10.8858026749064));
#23759=CARTESIAN_POINT('Ctrl Pts',(-0.318915406647834,-0.315184551632294,
11.0729748152654));
#23760=CARTESIAN_POINT('Ctrl Pts',(-0.952364882596371,-0.322700901737316,
10.9595743121341));
#23761=CARTESIAN_POINT('Ctrl Pts',(-1.46489024250333,-0.330217251842337,
10.5704271334521));
#23762=CARTESIAN_POINT('Ctrl Pts',(-1.74428917888433,-0.337733601947359,
9.99072509225252));
#23763=CARTESIAN_POINT('Ctrl Pts',(-1.72939530532362,-0.34524995205238,
9.34737812311678));
#23764=CARTESIAN_POINT('Ctrl Pts',(-1.42346960141787,-0.352766302157402,
8.78122563830929));
#23765=CARTESIAN_POINT('Ctrl Pts',(-0.893484683422232,-0.360282652262423,
8.41621556261918));
#23766=CARTESIAN_POINT('Ctrl Pts',(-0.255467131093149,-0.367799002367444,
8.33224436739279));
#23767=CARTESIAN_POINT('Ctrl Pts',(0.350911443806435,-0.375315352472466,
8.54772015826975));
#23768=CARTESIAN_POINT('Ctrl Pts',(0.792891925250241,-0.382831702577487,
9.01541553677525));
#23769=CARTESIAN_POINT('Ctrl Pts',(0.973726426719832,-0.390348052682509,
9.63305577615887));
#23770=CARTESIAN_POINT('Ctrl Pts',(0.893734635335651,-0.395358952752523,
10.0544460805015));
#23771=CARTESIAN_POINT('Ctrl Pts',(0.808000680481646,-0.39786440278753,
10.2446120463461));
#23772=CARTESIAN_POINT('Ctrl Pts',(-1.74047515456274,-0.153340700610567,
9.6));
#23773=CARTESIAN_POINT('Ctrl Pts',(-1.72473294771491,-0.155846150645574,
9.38897962842498));
#23774=CARTESIAN_POINT('Ctrl Pts',(-1.59182918820986,-0.160857050715588,
8.97467404719576));
#23775=CARTESIAN_POINT('Ctrl Pts',(-1.13137979800106,-0.16837340082061,
8.51185836372975));
#23776=CARTESIAN_POINT('Ctrl Pts',(-0.510855101828509,-0.175889750925631,
8.30921711856289));
#23777=CARTESIAN_POINT('Ctrl Pts',(0.133963800845887,-0.183406101030653,
8.41101677605048));
#23778=CARTESIAN_POINT('Ctrl Pts',(0.6618767398833,-0.190922451135674,8.79501556814522));
#23779=CARTESIAN_POINT('Ctrl Pts',(0.957328036294311,-0.198438801240695,
9.37712762811596));
#23780=CARTESIAN_POINT('Ctrl Pts',(0.955629869759482,-0.205955151345717,
10.0299261577517));
#23781=CARTESIAN_POINT('Ctrl Pts',(0.657157393790918,-0.213471501450738,
10.6104956232018));
#23782=CARTESIAN_POINT('Ctrl Pts',(0.127250814334077,-0.22098785155576,
10.9917394341285));
#23783=CARTESIAN_POINT('Ctrl Pts',(-0.51808163163464,-0.228504201660781,
11.0901944817538));
#23784=CARTESIAN_POINT('Ctrl Pts',(-1.13756367639728,-0.236020551765803,
10.8843073670163));
#23785=CARTESIAN_POINT('Ctrl Pts',(-1.59557773848644,-0.243536901870824,
10.4191508274041));
#23786=CARTESIAN_POINT('Ctrl Pts',(-1.79185514755587,-0.251053251975845,
9.79655733923979));
#23787=CARTESIAN_POINT('Ctrl Pts',(-1.68342668794294,-0.258569602080867,
9.15282543971024));
#23788=CARTESIAN_POINT('Ctrl Pts',(-1.29402960630127,-0.266085952185888,
8.62888136676785));
#23789=CARTESIAN_POINT('Ctrl Pts',(-0.708910964262916,-0.27360230229091,
8.3394272966268));
#23790=CARTESIAN_POINT('Ctrl Pts',(-0.0561653287950267,-0.281118652395931,
8.34783071254341));
#23791=CARTESIAN_POINT('Ctrl Pts',(0.521307791358451,-0.288635002500952,
8.65225192980931));
#23792=CARTESIAN_POINT('Ctrl Pts',(0.897087595000832,-0.296151352605974,
9.18604685593405));
#23793=CARTESIAN_POINT('Ctrl Pts',(0.988908116192752,-0.303667702710995,
9.83235674341108));
#23794=CARTESIAN_POINT('Ctrl Pts',(0.776667946887822,-0.311184052816017,
10.4496910125549));
#23795=CARTESIAN_POINT('Ctrl Pts',(0.306830842596235,-0.318700402921038,
10.9029024072114));
#23796=CARTESIAN_POINT('Ctrl Pts',(-0.317746135512149,-0.32621675302606,
11.0927736420849));
#23797=CARTESIAN_POINT('Ctrl Pts',(-0.960330197422347,-0.333733103131081,
10.9777378599246));
#23798=CARTESIAN_POINT('Ctrl Pts',(-1.48024637085961,-0.341249453236102,
10.5829790287109));
#23799=CARTESIAN_POINT('Ctrl Pts',(-1.7636743477543,-0.348765803341124,
9.99491746030589));
#23800=CARTESIAN_POINT('Ctrl Pts',(-1.74856569878764,-0.356282153446145,
9.34229317953619));
#23801=CARTESIAN_POINT('Ctrl Pts',(-1.43822842814087,-0.363798503551167,
8.76797655735667));
#23802=CARTESIAN_POINT('Ctrl Pts',(-0.900600923047711,-0.371314853656188,
8.39770289547719));
#23803=CARTESIAN_POINT('Ctrl Pts',(-0.253382911332231,-0.37883120376121,
8.31252080320183));
#23804=CARTESIAN_POINT('Ctrl Pts',(0.361739876686224,-0.386347553866231,
8.53110383815927));
#23805=CARTESIAN_POINT('Ctrl Pts',(0.810093887281791,-0.393863903971252,
9.0055435645584));
#23806=CARTESIAN_POINT('Ctrl Pts',(0.993536092066686,-0.401380254076274,
9.63209041460987));
#23807=CARTESIAN_POINT('Ctrl Pts',(0.912390788173031,-0.406391154146288,
10.0595573298025));
#23808=CARTESIAN_POINT('Ctrl Pts',(0.825420516595779,-0.408896604181295,
10.2524655622807));
#23809=CARTESIAN_POINT('',(0.938792124585917,-0.2,9.6));
#23810=CARTESIAN_POINT('',(0.882983735526293,-0.167820985845947,9.6));
#23811=CARTESIAN_POINT('Ctrl Pts',(0.938792124585917,-0.2,9.6));
#23812=CARTESIAN_POINT('Ctrl Pts',(0.92977267608958,-0.194799120566257,
9.6));
#23813=CARTESIAN_POINT('Ctrl Pts',(0.920750513898092,-0.189596807415628,
9.6));
#23814=CARTESIAN_POINT('Ctrl Pts',(0.902150020937586,-0.178871773266908,
9.6));
#23815=CARTESIAN_POINT('Ctrl Pts',(0.892565160581531,-0.17334530521579,
9.6));
#23816=CARTESIAN_POINT('Ctrl Pts',(0.882983735526293,-0.167820985845947,
9.6));
#23817=CARTESIAN_POINT('',(0.934663813609417,-0.2,9.8));
#23818=CARTESIAN_POINT('Ctrl Pts',(0.934605726336547,-0.2,9.80001655533327));
#23819=CARTESIAN_POINT('Ctrl Pts',(0.939837723241998,-0.2,9.74496032472243));
#23820=CARTESIAN_POINT('Ctrl Pts',(0.941679232433745,-0.2,9.689639007292));
#23821=CARTESIAN_POINT('Ctrl Pts',(0.940136539876103,-0.2,9.6343742241444));
#23822=CARTESIAN_POINT('Ctrl Pts',(0.939816429070574,-0.2,9.62290670641825));
#23823=CARTESIAN_POINT('Ctrl Pts',(0.939350427036596,-0.2,9.61144160667945));
#23824=CARTESIAN_POINT('Ctrl Pts',(0.938738309086801,-0.2,9.59998178926018));
#23825=CARTESIAN_POINT('',(0.882983735526293,-0.170296992535546,9.8));
#23826=CARTESIAN_POINT('Ctrl Pts',(0.882983735526293,-0.170296992535546,
9.8));
#23827=CARTESIAN_POINT('Ctrl Pts',(0.89256533649203,-0.175802996473857,
9.8));
#23828=CARTESIAN_POINT('Ctrl Pts',(0.902150185403708,-0.181311444968124,
9.8));
#23829=CARTESIAN_POINT('Ctrl Pts',(0.919374602560811,-0.191211354334495,
9.8));
#23830=CARTESIAN_POINT('Ctrl Pts',(0.927019922390104,-0.195605924238071,
9.8));
#23831=CARTESIAN_POINT('Ctrl Pts',(0.934663813609417,-0.2,9.8));
#23832=CARTESIAN_POINT('Ctrl Pts',(0.882930320251132,-0.170296992535546,
9.80001652754054));
#23833=CARTESIAN_POINT('Ctrl Pts',(0.877609657584953,-0.171150844078505,
9.86885824031965));
#23834=CARTESIAN_POINT('Ctrl Pts',(0.835029778105595,-0.17451014565647,
10.1379865677368));
#23835=CARTESIAN_POINT('Ctrl Pts',(0.612073665477375,-0.180374897269443,
10.5716664596844));
#23836=CARTESIAN_POINT('Ctrl Pts',(0.104765579300823,-0.187891247374464,
10.9366516770526));
#23837=CARTESIAN_POINT('Ctrl Pts',(-0.513045900691733,-0.195407597479486,
11.0309079926402));
#23838=CARTESIAN_POINT('Ctrl Pts',(-1.10610940043427,-0.202923947584507,
10.8338011775994));
#23839=CARTESIAN_POINT('Ctrl Pts',(-1.54459091073853,-0.210440297689529,
10.3884817891799));
#23840=CARTESIAN_POINT('Ctrl Pts',(-1.6790482842046,-0.215818644891609,
9.96198194106933));
#23841=CARTESIAN_POINT('Ctrl Pts',(-1.68694501923047,-0.218691542058681,
9.72972816411997));
#23842=CARTESIAN_POINT('Ctrl Pts',(-1.6869212373449,-0.219058989190747,
9.70002100226366));
#23843=CARTESIAN_POINT('',(-0.514332464396186,-0.3758,8.36074669039516));
#23844=CARTESIAN_POINT('Ctrl Pts',(-0.5143324643962,-0.3758,8.36074669039516));
#23845=CARTESIAN_POINT('Ctrl Pts',(-0.459186112744666,-0.3758,8.35715151017609));
#23846=CARTESIAN_POINT('Ctrl Pts',(-0.403937654194788,-0.3758,8.35693183338276));
#23847=CARTESIAN_POINT('Ctrl Pts',(-0.348901189845087,-0.3758,8.36012059653181));
#23848=CARTESIAN_POINT('Ctrl Pts',(-0.318949026847784,-0.3758,8.36185599786488));
#23849=CARTESIAN_POINT('Ctrl Pts',(-0.289059567473804,-0.3758,8.36460180455001));
#23850=CARTESIAN_POINT('Ctrl Pts',(-0.259283881757075,-0.3758,8.36836982212099));
#23851=CARTESIAN_POINT('Ctrl Pts',(-0.238690403378431,-0.3758,8.37097586079015));
#23852=CARTESIAN_POINT('Ctrl Pts',(-0.218151358285065,-0.3758,8.3740709655289));
#23853=CARTESIAN_POINT('Ctrl Pts',(-0.197682861612178,-0.3758,8.37764974829637));
#23854=CARTESIAN_POINT('Ctrl Pts',(-0.185643896254699,-0.3758,8.37975468264734));
#23855=CARTESIAN_POINT('Ctrl Pts',(-0.173627293719959,-0.3758,8.3820273824134));
#23856=CARTESIAN_POINT('Ctrl Pts',(-0.161642970436637,-0.3758,8.38446555730322));
#23857=CARTESIAN_POINT('Ctrl Pts',(-0.107637690513597,-0.3758,8.39545277070804));
#23858=CARTESIAN_POINT('Ctrl Pts',(-0.0544133015938191,-0.3758,8.40976919406099));
#23859=CARTESIAN_POINT('Ctrl Pts',(-0.00226237454520876,-0.3758,8.42727966409744));
#23860=CARTESIAN_POINT('Ctrl Pts',(0.030941959568332,-0.3758,8.43842852626499));
#23861=CARTESIAN_POINT('Ctrl Pts',(0.0637110029072512,-0.3758,8.45087327629095));
#23862=CARTESIAN_POINT('Ctrl Pts',(0.0959655247076156,-0.3758,8.46458937152845));
#23863=CARTESIAN_POINT('Ctrl Pts',(0.115792643065664,-0.3758,8.47302076745388));
#23864=CARTESIAN_POINT('Ctrl Pts',(0.135425272733956,-0.3758,8.48193271440877));
#23865=CARTESIAN_POINT('Ctrl Pts',(0.154844151472763,-0.3758,8.49132089519076));
#23866=CARTESIAN_POINT('Ctrl Pts',(0.164400066961461,-0.3758,8.49594076348243));
#23867=CARTESIAN_POINT('Ctrl Pts',(0.173903375406978,-0.3758,8.5006756813438));
#23868=CARTESIAN_POINT('Ctrl Pts',(0.18334038592269,-0.3758,8.50551899364961));
#23869=CARTESIAN_POINT('Ctrl Pts',(0.231990305124483,-0.3758,8.53048736175241));
#23870=CARTESIAN_POINT('Ctrl Pts',(0.278961911005049,-0.3758,8.55837168896474));
#23871=CARTESIAN_POINT('Ctrl Pts',(0.323970100024214,-0.3758,8.58905342668914));
#23872=CARTESIAN_POINT('Ctrl Pts',(0.369162236320362,-0.3758,8.61986055986335));
#23873=CARTESIAN_POINT('Ctrl Pts',(0.41237579564963,-0.3758,8.6534885441088));
#23874=CARTESIAN_POINT('Ctrl Pts',(0.453401593903601,-0.3758,8.68969605386198));
#23875=CARTESIAN_POINT('Ctrl Pts',(0.482061638209065,-0.3758,8.71499010974586));
#23876=CARTESIAN_POINT('Ctrl Pts',(0.509653403937738,-0.3758,8.74154398427469));
#23877=CARTESIAN_POINT('Ctrl Pts',(0.536094141849884,-0.3758,8.76928524079275));
#23878=CARTESIAN_POINT('Ctrl Pts',(0.545597327910121,-0.3758,8.77925585216947));
#23879=CARTESIAN_POINT('Ctrl Pts',(0.554951726191651,-0.3758,8.78937991159023));
#23880=CARTESIAN_POINT('Ctrl Pts',(0.564153143107668,-0.3758,8.79965425101923));
#23881=CARTESIAN_POINT('Ctrl Pts',(0.570667013019575,-0.3758,8.8069276645687));
#23882=CARTESIAN_POINT('Ctrl Pts',(0.577103878399466,-0.3758,8.814276170528));
#23883=CARTESIAN_POINT('Ctrl Pts',(0.583453562357181,-0.3758,8.82168809871078));
#23884=CARTESIAN_POINT('Ctrl Pts',(0.618945997994518,-0.3758,8.8631180951843));
#23885=CARTESIAN_POINT('Ctrl Pts',(0.651791132138043,-0.3758,8.90660779224594));
#23886=CARTESIAN_POINT('Ctrl Pts',(0.681792858457505,-0.3758,8.95191277562012));
#23887=CARTESIAN_POINT('Ctrl Pts',(0.70212728285197,-0.3758,8.98261936727772));
#23888=CARTESIAN_POINT('Ctrl Pts',(0.721154825564954,-0.3758,9.014160730134));
#23889=CARTESIAN_POINT('Ctrl Pts',(0.738803455298371,-0.3758,9.04646884572015));
#23890=CARTESIAN_POINT('Ctrl Pts',(0.763421765357715,-0.3758,9.09153586899318));
#23891=CARTESIAN_POINT('Ctrl Pts',(0.78535872190006,-0.3758,9.13809472230648));
#23892=CARTESIAN_POINT('Ctrl Pts',(0.804529778979719,-0.3758,9.18588977192258));
#23893=CARTESIAN_POINT('Ctrl Pts',(0.80997310737791,-0.3758,9.1994604451404));
#23894=CARTESIAN_POINT('Ctrl Pts',(0.815193201908606,-0.3758,9.21313083794842));
#23895=CARTESIAN_POINT('Ctrl Pts',(0.820187520955781,-0.3758,9.22689519764528));
#23896=CARTESIAN_POINT('Ctrl Pts',(0.824722129234267,-0.3758,9.2393925929538));
#23897=CARTESIAN_POINT('Ctrl Pts',(0.829071936284644,-0.3758,9.25197198301473));
#23898=CARTESIAN_POINT('Ctrl Pts',(0.833226054633313,-0.3758,9.26460086536546));
#23899=CARTESIAN_POINT('Ctrl Pts',(0.850147611958222,-0.3758,9.31604387654393));
#23900=CARTESIAN_POINT('Ctrl Pts',(0.863857203739219,-0.3758,9.36838576470231));
#23901=CARTESIAN_POINT('Ctrl Pts',(0.87429910262014,-0.3758,9.42131543047171));
#23902=CARTESIAN_POINT('Ctrl Pts',(0.884689718113437,-0.3758,9.47398514231917));
#23903=CARTESIAN_POINT('Ctrl Pts',(0.891844862197499,-0.3758,9.52723792662456));
#23904=CARTESIAN_POINT('Ctrl Pts',(0.895659916756747,-0.3758,9.58077807753031));
#23905=CARTESIAN_POINT('Ctrl Pts',(0.896985769943157,-0.3758,9.59938498827741));
#23906=CARTESIAN_POINT('Ctrl Pts',(0.897907756370869,-0.3758,9.61802662991583));
#23907=CARTESIAN_POINT('Ctrl Pts',(0.898419996116996,-0.3758,9.63669054313271));
#23908=CARTESIAN_POINT('Ctrl Pts',(0.89914203714867,-0.3758,9.66299875380179));
#23909=CARTESIAN_POINT('Ctrl Pts',(0.899050055209692,-0.3758,9.68935126075387));
#23910=CARTESIAN_POINT('Ctrl Pts',(0.898148036015986,-0.3758,9.71571189798373));
#23911=CARTESIAN_POINT('Ctrl Pts',(0.897793169615475,-0.3758,9.72608252481098));
#23912=CARTESIAN_POINT('Ctrl Pts',(0.897312803258196,-0.3758,9.73645602369309));
#23913=CARTESIAN_POINT('Ctrl Pts',(0.896707362381433,-0.3758,9.74682507694203));
#23914=CARTESIAN_POINT('Ctrl Pts',(0.893575068153731,-0.3758,9.80047015920346));
#23915=CARTESIAN_POINT('Ctrl Pts',(0.887113972407378,-0.3758,9.85376450073757));
#23916=CARTESIAN_POINT('Ctrl Pts',(0.877430475724668,-0.3758,9.90640969563552));
#23917=CARTESIAN_POINT('Ctrl Pts',(0.86771391187951,-0.3758,9.95923466311653));
#23918=CARTESIAN_POINT('Ctrl Pts',(0.854752661161743,-0.3758,10.0114071099657));
#23919=CARTESIAN_POINT('Ctrl Pts',(0.838602504381783,-0.3758,10.0626183118125));
#23920=CARTESIAN_POINT('Ctrl Pts',(0.822752772426385,-0.3758,10.112876884125));
#23921=CARTESIAN_POINT('Ctrl Pts',(0.803831305864454,-0.3758,10.1622105740949));
#23922=CARTESIAN_POINT('Ctrl Pts',(0.781845869462943,-0.3758,10.2103058753372));
#23923=CARTESIAN_POINT('Ctrl Pts',(0.77900224348841,-0.3758,10.2165265864191));
#23924=CARTESIAN_POINT('Ctrl Pts',(0.776107301341429,-0.3758,10.2227265387929));
#23925=CARTESIAN_POINT('Ctrl Pts',(0.773161008253381,-0.3758,10.228905014477));
#23926=CARTESIAN_POINT('Ctrl Pts',(-1.74411350535466,-0.352155593372042,
9.70000771515446));
#23927=CARTESIAN_POINT('Ctrl Pts',(-1.74408777242683,-0.353531113396743,
9.58381303222107));
#23928=CARTESIAN_POINT('Ctrl Pts',(-1.72913983536605,-0.354906633421444,
9.46761183026196));
#23929=CARTESIAN_POINT('Ctrl Pts',(-1.69936092850762,-0.356282153446145,
9.35534445596789));
#23930=CARTESIAN_POINT('Ctrl Pts',(-1.64511994190538,-0.358787603481153,
9.15085430547635));
#23931=CARTESIAN_POINT('Ctrl Pts',(-1.54167418502313,-0.36129305351616,
8.95941543141651));
#23932=CARTESIAN_POINT('Ctrl Pts',(-1.40034672239981,-0.363798503551167,
8.80198371740668));
#23933=CARTESIAN_POINT('Ctrl Pts',(-1.25901925977648,-0.366303953586174,
8.64455200339684));
#23934=CARTESIAN_POINT('Ctrl Pts',(-1.0798100914121,-0.368809403621181,
8.52112744943702));
#23935=CARTESIAN_POINT('Ctrl Pts',(-0.882335838610658,-0.371314853656188,
8.44521815707788));
#23936=CARTESIAN_POINT('Ctrl Pts',(-0.764499267592279,-0.372809902437459,
8.39992166605114));
#23937=CARTESIAN_POINT('Ctrl Pts',(-0.64015899031043,-0.374304951218729,
8.37154408418945));
#23938=CARTESIAN_POINT('Ctrl Pts',(-0.514332464396186,-0.3758,8.36074669039516));
#23939=CARTESIAN_POINT('',(-1.70717578408079,-0.134200000000245,9.59999999967343));
#23940=CARTESIAN_POINT('Ctrl Pts',(-1.70717578408079,-0.134200000000245,
9.59999999967343));
#23941=CARTESIAN_POINT('Ctrl Pts',(-1.70869435368597,-0.135072786034822,
9.59999999967343));
#23942=CARTESIAN_POINT('Ctrl Pts',(-1.71021285656339,-0.135945547417202,
9.6));
#23943=CARTESIAN_POINT('Ctrl Pts',(-1.72131168622386,-0.14232471291867,
9.6));
#23944=CARTESIAN_POINT('Ctrl Pts',(-1.73089522164145,-0.147833488670363,
9.6));
#23945=CARTESIAN_POINT('Ctrl Pts',(-1.74047515456274,-0.153340700610567,
9.6));
#23946=CARTESIAN_POINT('',(-1.14715243039944,-0.134200000000245,8.65223546950032));
#23947=CARTESIAN_POINT('Ctrl Pts',(-1.14715616136387,-0.134200000000245,
8.65218366173329));
#23948=CARTESIAN_POINT('Ctrl Pts',(-1.1914614130295,-0.134200000000245,
8.68241986696621));
#23949=CARTESIAN_POINT('Ctrl Pts',(-1.23378474695924,-0.134200000000245,
8.71538107777202));
#23950=CARTESIAN_POINT('Ctrl Pts',(-1.27392321752278,-0.134200000000245,
8.75081519069846));
#23951=CARTESIAN_POINT('Ctrl Pts',(-1.30598751675522,-0.134200000000245,
8.77912145110046));
#23952=CARTESIAN_POINT('Ctrl Pts',(-1.33665733147895,-0.134200000000245,
8.80900694133707));
#23953=CARTESIAN_POINT('Ctrl Pts',(-1.36581520383624,-0.134200000000245,
8.84036234914257));
#23954=CARTESIAN_POINT('Ctrl Pts',(-1.37659359337313,-0.134200000000245,
8.85195307137615));
#23955=CARTESIAN_POINT('Ctrl Pts',(-1.38716523755777,-0.134200000000245,
8.86374479838921));
#23956=CARTESIAN_POINT('Ctrl Pts',(-1.39752365245874,-0.134200000000245,
8.87573248846776));
#23957=CARTESIAN_POINT('Ctrl Pts',(-1.40511942403085,-0.134200000000245,
8.88452299902217));
#23958=CARTESIAN_POINT('Ctrl Pts',(-1.41259434273687,-0.134200000000245,
8.89341174311036));
#23959=CARTESIAN_POINT('Ctrl Pts',(-1.41994559115476,-0.134200000000245,
8.90239537788468));
#23960=CARTESIAN_POINT('Ctrl Pts',(-1.45199276022031,-0.134200000000245,
8.94155880239023));
#23961=CARTESIAN_POINT('Ctrl Pts',(-1.48169668421176,-0.134200000000245,
8.9825288838409));
#23962=CARTESIAN_POINT('Ctrl Pts',(-1.508870618509,-0.134200000000245,9.02512022251993));
#23963=CARTESIAN_POINT('Ctrl Pts',(-1.52582288453517,-0.134200000000245,
9.05169052683433));
#23964=CARTESIAN_POINT('Ctrl Pts',(-1.54178999378989,-0.134200000000245,
9.0788923978278));
#23965=CARTESIAN_POINT('Ctrl Pts',(-1.5567543716842,-0.134200000000245,
9.10666559889433));
#23966=CARTESIAN_POINT('Ctrl Pts',(-1.56527812592892,-0.134200000000245,
9.12248529699018));
#23967=CARTESIAN_POINT('Ctrl Pts',(-1.57347645003769,-0.134200000000245,
9.13849042183118));
#23968=CARTESIAN_POINT('Ctrl Pts',(-1.58134529711494,-0.134200000000245,
9.15467023201953));
#23969=CARTESIAN_POINT('Ctrl Pts',(-1.58594460208478,-0.134200000000245,
9.16412725675007));
#23970=CARTESIAN_POINT('Ctrl Pts',(-1.59042915639314,-0.134200000000245,
9.17363962921911));
#23971=CARTESIAN_POINT('Ctrl Pts',(-1.59479527804768,-0.134200000000245,
9.18319785476236));
#23972=CARTESIAN_POINT('Ctrl Pts',(-1.61725813407457,-0.134200000000245,
9.23237308652148));
#23973=CARTESIAN_POINT('Ctrl Pts',(-1.63661737531215,-0.134200000000245,
9.2828161835826));
#23974=CARTESIAN_POINT('Ctrl Pts',(-1.65281487649832,-0.134200000000245,
9.33421256568847));
#23975=CARTESIAN_POINT('Ctrl Pts',(-1.66903680873791,-0.134200000000245,
9.38568647010737));
#23976=CARTESIAN_POINT('Ctrl Pts',(-1.68208782495732,-0.134200000000244,
9.43811754687342));
#23977=CARTESIAN_POINT('Ctrl Pts',(-1.6918629726923,-0.134200000000244,
9.49121192885304));
#23978=CARTESIAN_POINT('Ctrl Pts',(-1.69848855151139,-0.134200000000244,
9.52719921233908));
#23979=CARTESIAN_POINT('Ctrl Pts',(-1.70360819823688,-0.134200000000244,
9.56349167464818));
#23980=CARTESIAN_POINT('Ctrl Pts',(-1.70717574316321,-0.134200000000244,
9.60000000632835));
#23981=CARTESIAN_POINT('Ctrl Pts',(-1.14715616136387,-0.134200000000245,
8.65218366173329));
#23982=CARTESIAN_POINT('Ctrl Pts',(-1.12354250101448,-0.134558932213268,
8.63531594196993));
#23983=CARTESIAN_POINT('Ctrl Pts',(-0.930537218441067,-0.137423314461298,
8.50712576737122));
#23984=CARTESIAN_POINT('Ctrl Pts',(-0.506127554802531,-0.142793146744336,
8.36852870067744));
#23985=CARTESIAN_POINT('Ctrl Pts',(0.111192282557321,-0.150309496849357,
8.46598699128103));
#23986=CARTESIAN_POINT('Ctrl Pts',(0.616591749469812,-0.157825846954379,
8.83360970038453));
#23987=CARTESIAN_POINT('Ctrl Pts',(0.836252869028476,-0.163663009953242,
9.26639638419685));
#23988=CARTESIAN_POINT('Ctrl Pts',(0.877788525907663,-0.166994722917098,
9.53336507663716));
#23989=CARTESIAN_POINT('Ctrl Pts',(0.882934918736163,-0.167820985845947,
9.59998192031225));
#23990=CARTESIAN_POINT('Origin',(-0.4,-0.134200000000245,9.7));
#23991=CARTESIAN_POINT('',(0.940475154562985,-0.134200000000245,9.8));
#23992=CARTESIAN_POINT('',(0.911390797333273,-0.134200000000245,9.80000000017706));
#23993=CARTESIAN_POINT('',(0.3,-0.134200000000245,9.8));
#23994=CARTESIAN_POINT('',(0.175723864053005,-0.134200000000245,10.9146668976966));
#23995=CARTESIAN_POINT('Origin',(-0.4,-0.1342,9.7));
#23996=CARTESIAN_POINT('Ctrl Pts',(0.176129947875695,-0.134200000000245,
10.9150835725709));
#23997=CARTESIAN_POINT('Ctrl Pts',(0.198206219307209,-0.134200000000245,
10.9040341608737));
#23998=CARTESIAN_POINT('Ctrl Pts',(0.219948760930549,-0.134200000000245,
10.8923781854623));
#23999=CARTESIAN_POINT('Ctrl Pts',(0.241329692205113,-0.134200000000245,
10.8801261273095));
#24000=CARTESIAN_POINT('Ctrl Pts',(0.289254661940267,-0.134200000000245,
10.852663361136));
#24001=CARTESIAN_POINT('Ctrl Pts',(0.335364934801413,-0.134200000000245,
10.8222085932717));
#24002=CARTESIAN_POINT('Ctrl Pts',(0.37946815304655,-0.134200000000245,
10.7890106425309));
#24003=CARTESIAN_POINT('Ctrl Pts',(0.408853584657123,-0.134200000000245,
10.7668912564653));
#24004=CARTESIAN_POINT('Ctrl Pts',(0.437347467573836,-0.134200000000245,
10.7435530764034));
#24005=CARTESIAN_POINT('Ctrl Pts',(0.464884284027698,-0.134200000000245,
10.7190603557891));
#24006=CARTESIAN_POINT('Ctrl Pts',(0.473497528744165,-0.134200000000245,
10.7113992742412));
#24007=CARTESIAN_POINT('Ctrl Pts',(0.482009956489796,-0.134200000000245,
10.7036315198068));
#24008=CARTESIAN_POINT('Ctrl Pts',(0.490419673663885,-0.134200000000245,
10.695759684914));
#24009=CARTESIAN_POINT('Ctrl Pts',(0.530763113022545,-0.134200000000245,
10.6579965964454));
#24010=CARTESIAN_POINT('Ctrl Pts',(0.568747696285602,-0.134200000000245,
10.6178394709025));
#24011=CARTESIAN_POINT('Ctrl Pts',(0.604171126971739,-0.134200000000245,
10.5755260135067));
#24012=CARTESIAN_POINT('Ctrl Pts',(0.626117013454232,-0.134200000000245,
10.5493115471294));
#24013=CARTESIAN_POINT('Ctrl Pts',(0.647079204216221,-0.134200000000245,
10.5222686612886));
#24014=CARTESIAN_POINT('Ctrl Pts',(0.667001543377484,-0.134200000000245,
10.4944478859121));
#24015=CARTESIAN_POINT('Ctrl Pts',(0.675322521123416,-0.134200000000245,
10.4828279626236));
#24016=CARTESIAN_POINT('Ctrl Pts',(0.6834620162914,-0.134200000000245,10.4710722913384));
#24017=CARTESIAN_POINT('Ctrl Pts',(0.691415568045136,-0.134200000000245,
10.4591843752824));
#24018=CARTESIAN_POINT('Ctrl Pts',(0.6977908946228,-0.134200000000245,10.4496553812516));
#24019=CARTESIAN_POINT('Ctrl Pts',(0.704042066980966,-0.134200000000245,
10.4400483233876));
#24020=CARTESIAN_POINT('Ctrl Pts',(0.710164383835293,-0.134200000000245,
10.4303700616719));
#24021=CARTESIAN_POINT('Ctrl Pts',(0.739480248268273,-0.134200000000245,
10.3840270488624));
#24022=CARTESIAN_POINT('Ctrl Pts',(0.765867642510717,-0.134200000000245,
10.3360201025942));
#24023=CARTESIAN_POINT('Ctrl Pts',(0.789126895014165,-0.134200000000245,
10.2865747717069));
#24024=CARTESIAN_POINT('Ctrl Pts',(0.798476858430171,-0.134200000000245,
10.2666982930961));
#24025=CARTESIAN_POINT('Ctrl Pts',(0.807320848203325,-0.134200000000245,
10.2465890474885));
#24026=CARTESIAN_POINT('Ctrl Pts',(0.815643802636578,-0.134200000000245,
10.226260533697));
#24027=CARTESIAN_POINT('Ctrl Pts',(0.836342359052429,-0.134200000000245,
10.1757050617263));
#24028=CARTESIAN_POINT('Ctrl Pts',(0.853822018600959,-0.134200000000245,
10.1237940561666));
#24029=CARTESIAN_POINT('Ctrl Pts',(0.868036229685716,-0.134200000000245,
10.0708733149591));
#24030=CARTESIAN_POINT('Ctrl Pts',(0.874996360496826,-0.134200000000245,
10.0449601440325));
#24031=CARTESIAN_POINT('Ctrl Pts',(0.881172765951885,-0.134200000000245,
10.0188047170997));
#24032=CARTESIAN_POINT('Ctrl Pts',(0.886555417284674,-0.134200000000245,
9.9924474119145));
#24033=CARTESIAN_POINT('Ctrl Pts',(0.888524749963501,-0.134200000000245,
9.98280415263246));
#24034=CARTESIAN_POINT('Ctrl Pts',(0.890387666143772,-0.134200000000245,
9.97313401876206));
#24035=CARTESIAN_POINT('Ctrl Pts',(0.892141380051336,-0.134200000000245,
9.9634529226972));
#24036=CARTESIAN_POINT('Ctrl Pts',(0.901950899807882,-0.134200000000245,
9.90930104381685));
#24037=CARTESIAN_POINT('Ctrl Pts',(0.90837109872301,-0.134200000000245,
9.85469798328913));
#24038=CARTESIAN_POINT('Ctrl Pts',(0.911390797333273,-0.134200000000245,
9.80000000035412));
#24039=CARTESIAN_POINT('Origin',(-0.4,-0.134200000000245,9.7));
#24040=CARTESIAN_POINT('',(-1.74047515456298,-0.134200000000245,9.6));
#24041=CARTESIAN_POINT('',(-1.1,-0.134200000000245,9.6));
#24042=CARTESIAN_POINT('',(0.940475154562985,-0.134200000000245,9.6));
#24043=CARTESIAN_POINT('Origin',(-0.4,-0.1342,9.7));
#24044=CARTESIAN_POINT('',(0.907175784144596,-0.134200000000245,9.6));
#24045=CARTESIAN_POINT('',(0.1,-0.134200000000245,9.6));
#24046=CARTESIAN_POINT('',(0.347152430399435,-0.134200000000245,8.65223546950032));
#24047=CARTESIAN_POINT('Ctrl Pts',(0.907175784144597,-0.134200000000245,
9.6));
#24048=CARTESIAN_POINT('Ctrl Pts',(0.90453538373471,-0.134200000000245,
9.57297027207912));
#24049=CARTESIAN_POINT('Ctrl Pts',(0.901034611734171,-0.134200000000245,
9.54600708743907));
#24050=CARTESIAN_POINT('Ctrl Pts',(0.896684152486396,-0.134200000000245,
9.51914778346216));
#24051=CARTESIAN_POINT('Ctrl Pts',(0.894686994277047,-0.134200000000245,
9.50681752672838));
#24052=CARTESIAN_POINT('Ctrl Pts',(0.892510728072362,-0.134200000000245,
9.49450917871624));
#24053=CARTESIAN_POINT('Ctrl Pts',(0.890156179963373,-0.134200000000245,
9.48222644915194));
#24054=CARTESIAN_POINT('Ctrl Pts',(0.888356131663543,-0.134200000000245,
9.47283632185529));
#24055=CARTESIAN_POINT('Ctrl Pts',(0.886452039893565,-0.134200000000245,
9.46346246266868));
#24056=CARTESIAN_POINT('Ctrl Pts',(0.884447124139638,-0.134200000000245,
9.45411839321025));
#24057=CARTESIAN_POINT('Ctrl Pts',(0.873091127340333,-0.134200000000245,
9.40119286621262));
#24058=CARTESIAN_POINT('Ctrl Pts',(0.858485365062411,-0.134200000000245,
9.34911826627378));
#24059=CARTESIAN_POINT('Ctrl Pts',(0.840774482262135,-0.134200000000245,
9.29817408776324));
#24060=CARTESIAN_POINT('Ctrl Pts',(0.823034248341469,-0.134200000000245,
9.24714548270357));
#24061=CARTESIAN_POINT('Ctrl Pts',(0.802178189415309,-0.134200000000245,
9.19725004063387));
#24062=CARTESIAN_POINT('Ctrl Pts',(0.778302217753888,-0.134200000000245,
9.14878475269468));
#24063=CARTESIAN_POINT('Ctrl Pts',(0.765046152196193,-0.134200000000245,
9.12187656888106));
#24064=CARTESIAN_POINT('Ctrl Pts',(0.750858347126933,-0.134200000000245,
9.09540960660686));
#24065=CARTESIAN_POINT('Ctrl Pts',(0.735749330922162,-0.134200000000245,
9.06943858140765));
#24066=CARTESIAN_POINT('Ctrl Pts',(0.726441613647345,-0.134200000000245,
9.05343946163604));
#24067=CARTESIAN_POINT('Ctrl Pts',(0.716784215230823,-0.134200000000245,
9.03762861234457));
#24068=CARTESIAN_POINT('Ctrl Pts',(0.706778867696372,-0.134200000000245,
9.02201952100148));
#24069=CARTESIAN_POINT('Ctrl Pts',(0.700542750909446,-0.134200000000245,
9.01229071186036));
#24070=CARTESIAN_POINT('Ctrl Pts',(0.694169554623091,-0.134200000000245,
9.00263770564262));
#24071=CARTESIAN_POINT('Ctrl Pts',(0.687672487303354,-0.134200000000245,
8.99308223011669));
#24072=CARTESIAN_POINT('Ctrl Pts',(0.657566969896279,-0.134200000000245,
8.94880493997611));
#24073=CARTESIAN_POINT('Ctrl Pts',(0.624758329671486,-0.134200000000245,
8.90654250878312));
#24074=CARTESIAN_POINT('Ctrl Pts',(0.589505146468692,-0.134200000000245,
8.86648555649876));
#24075=CARTESIAN_POINT('Ctrl Pts',(0.553825294071344,-0.134200000000245,
8.8259437950138));
#24076=CARTESIAN_POINT('Ctrl Pts',(0.51564061185778,-0.134200000000245,
8.78766039574739));
#24077=CARTESIAN_POINT('Ctrl Pts',(0.4751780594968,-0.134200000000245,8.75186738885961));
#24078=CARTESIAN_POINT('Ctrl Pts',(0.434715507135821,-0.134200000000245,
8.71607438197183));
#24079=CARTESIAN_POINT('Ctrl Pts',(0.391974258638634,-0.134200000000245,
8.68277097560167));
#24080=CARTESIAN_POINT('Ctrl Pts',(0.347152430399435,-0.134200000000245,
8.65223546950032));
#24081=CARTESIAN_POINT('Origin',(-0.4,-0.134200000000245,9.7));
#24082=CARTESIAN_POINT('Origin',(-0.4,-0.134200000000245,9.7));
#24083=CARTESIAN_POINT('',(-1.71139079735282,-0.134200000000245,9.8));
#24084=CARTESIAN_POINT('',(-1.74047515456298,-0.134200000000245,9.8));
#24085=CARTESIAN_POINT('',(-0.9,-0.134200000000245,9.8));
#24086=CARTESIAN_POINT('',(-0.975723864053004,-0.134200000000245,10.9146668976966));
#24087=CARTESIAN_POINT('Ctrl Pts',(-1.71139075641017,-0.134200000000245,
9.79999999241229));
#24088=CARTESIAN_POINT('Ctrl Pts',(-1.70840546976856,-0.134200000000245,
9.85403729104872));
#24089=CARTESIAN_POINT('Ctrl Pts',(-1.70201613810188,-0.134200000000245,
9.90781112718742));
#24090=CARTESIAN_POINT('Ctrl Pts',(-1.69235366903268,-0.134200000000245,
9.96103460131166));
#24091=CARTESIAN_POINT('Ctrl Pts',(-1.68443878317439,-0.134200000000245,
10.0046319178627));
#24092=CARTESIAN_POINT('Ctrl Pts',(-1.67432659504433,-0.134200000000245,
10.0478603021159));
#24093=CARTESIAN_POINT('Ctrl Pts',(-1.66206395378842,-0.134200000000245,
10.0905578444579));
#24094=CARTESIAN_POINT('Ctrl Pts',(-1.65801320249372,-0.134200000000245,
10.1046622385532));
#24095=CARTESIAN_POINT('Ctrl Pts',(-1.65372761924944,-0.134200000000245,
10.1187086493849));
#24096=CARTESIAN_POINT('Ctrl Pts',(-1.64920838417779,-0.134200000000245,
10.1326910333634));
#24097=CARTESIAN_POINT('Ctrl Pts',(-1.64492382198282,-0.134200000000245,
10.1459473461773));
#24098=CARTESIAN_POINT('Ctrl Pts',(-1.64042721171054,-0.134200000000245,
10.1591513010999));
#24099=CARTESIAN_POINT('Ctrl Pts',(-1.63573065417228,-0.134200000000245,
10.1722675160761));
#24100=CARTESIAN_POINT('Ctrl Pts',(-1.61716981388927,-0.134200000000245,
10.2241029230326));
#24101=CARTESIAN_POINT('Ctrl Pts',(-1.59546815140804,-0.134200000000245,
10.2746456376427));
#24102=CARTESIAN_POINT('Ctrl Pts',(-1.57076076646457,-0.134200000000245,
10.3236030074615));
#24103=CARTESIAN_POINT('Ctrl Pts',(-1.54842667430624,-0.134200000000245,
10.3678577277349));
#24104=CARTESIAN_POINT('Ctrl Pts',(-1.52363570557235,-0.134200000000245,
10.4108175770067));
#24105=CARTESIAN_POINT('Ctrl Pts',(-1.49645283004384,-0.134200000000245,
10.4522549727563));
#24106=CARTESIAN_POINT('Ctrl Pts',(-1.4664160175259,-0.134200000000245,
10.4980428911851));
#24107=CARTESIAN_POINT('Ctrl Pts',(-1.43345876263302,-0.134200000000245,
10.5419730627871));
#24108=CARTESIAN_POINT('Ctrl Pts',(-1.39780718339101,-0.134200000000245,
10.5838327068653));
#24109=CARTESIAN_POINT('Ctrl Pts',(-1.3893242475541,-0.134200000000245,
10.5937927894878));
#24110=CARTESIAN_POINT('Ctrl Pts',(-1.38068569252885,-0.134200000000245,
10.6036384832782));
#24111=CARTESIAN_POINT('Ctrl Pts',(-1.37191344138273,-0.134200000000245,
10.6133460664041));
#24112=CARTESIAN_POINT('Ctrl Pts',(-1.33495351450469,-0.134200000000245,
10.6542468063073));
#24113=CARTESIAN_POINT('Ctrl Pts',(-1.29556659195931,-0.134200000000245,
10.6927686437194));
#24114=CARTESIAN_POINT('Ctrl Pts',(-1.25402535771013,-0.134200000000245,
10.7287345588468));
#24115=CARTESIAN_POINT('Ctrl Pts',(-1.21177760165103,-0.134200000000245,
10.7653121723003));
#24116=CARTESIAN_POINT('Ctrl Pts',(-1.16730090284931,-0.134200000000245,
10.7992470464879));
#24117=CARTESIAN_POINT('Ctrl Pts',(-1.12084074134493,-0.134200000000245,
10.8303173024355));
#24118=CARTESIAN_POINT('Ctrl Pts',(-1.07438057984054,-0.134200000000245,
10.8613875583832));
#24119=CARTESIAN_POINT('Ctrl Pts',(-1.0259361067866,-0.134200000000245,
10.889594012123));
#24120=CARTESIAN_POINT('Ctrl Pts',(-0.975723864053004,-0.134200000000245,
10.9146668976966));
#24121=CARTESIAN_POINT('Origin',(-0.4,-0.1342,9.7));
#24122=CARTESIAN_POINT('Ctrl Pts',(-1.74304790533427,-0.166903395818705,
9.64435861273087));
#24123=CARTESIAN_POINT('Ctrl Pts',(-1.73435369961947,-0.169390260154196,
9.43450160975334));
#24124=CARTESIAN_POINT('Ctrl Pts',(-1.61686806594084,-0.17436398882518,
9.01909689256477));
#24125=CARTESIAN_POINT('Ctrl Pts',(-1.17795239257679,-0.181824581831654,
8.54274435715143));
#24126=CARTESIAN_POINT('Ctrl Pts',(-0.571227429489255,-0.189285174838129,
8.31612744124815));
#24127=CARTESIAN_POINT('Ctrl Pts',(0.0724614243232401,-0.196745767844604,
8.38804338598779));
#24128=CARTESIAN_POINT('Ctrl Pts',(0.6142113106438,-0.204206360851079,8.74302009654901));
#24129=CARTESIAN_POINT('Ctrl Pts',(0.93715526549064,-0.211666953857554,
9.30445338949781));
#24130=CARTESIAN_POINT('Ctrl Pts',(0.97161381549785,-0.219127546864028,
9.95122650445237));
#24131=CARTESIAN_POINT('Ctrl Pts',(0.710155473394963,-0.226588139870503,
10.5437975996746));
#24132=CARTESIAN_POINT('Ctrl Pts',(0.209187076810929,-0.234048732876978,
10.9543248434144));
#24133=CARTESIAN_POINT('Ctrl Pts',(-0.423209735858731,-0.241509325883453,
11.0942384369162));
#24134=CARTESIAN_POINT('Ctrl Pts',(-1.05059926803272,-0.248969918889928,
10.9333532476513));
#24135=CARTESIAN_POINT('Ctrl Pts',(-1.53762571409255,-0.256430511896403,
10.5063791358829));
#24136=CARTESIAN_POINT('Ctrl Pts',(-1.77921598078853,-0.263891104902878,
9.90543339520114));
#24137=CARTESIAN_POINT('Ctrl Pts',(-1.72324833240949,-0.271351697909352,
9.26016657257637));
#24138=CARTESIAN_POINT('Ctrl Pts',(-1.38179747864361,-0.278812290915827,
8.70979127833806));
#24139=CARTESIAN_POINT('Ctrl Pts',(-0.828529470919906,-0.286272883922302,
8.373047827273));
#24140=CARTESIAN_POINT('Ctrl Pts',(-0.18280869586118,-0.293733476928777,
8.32258663486116));
#24141=CARTESIAN_POINT('Ctrl Pts',(0.416054301607959,-0.301194069935252,
8.56929451772788));
#24142=CARTESIAN_POINT('Ctrl Pts',(0.838858292162744,-0.308654662941726,
9.05994544037276));
#24143=CARTESIAN_POINT('Ctrl Pts',(0.994385717937961,-0.316115255948201,
9.68868479182157));
#24144=CARTESIAN_POINT('Ctrl Pts',(0.849082503222856,-0.323575848954676,
10.3198645945257));
#24145=CARTESIAN_POINT('Ctrl Pts',(0.434296837286034,-0.331036441961151,
10.8173137931681));
#24146=CARTESIAN_POINT('Ctrl Pts',(-0.160483306787659,-0.338497034967626,
11.0737055259114));
#24147=CARTESIAN_POINT('Ctrl Pts',(-0.806938123001907,-0.345957627974101,
11.0337358503735));
#24148=CARTESIAN_POINT('Ctrl Pts',(-1.36559670937883,-0.353418220980575,
10.7060045160499));
#24149=CARTESIAN_POINT('Ctrl Pts',(-1.71593306059597,-0.36087881398705,
10.1612707751975));
#24150=CARTESIAN_POINT('Ctrl Pts',(-1.78234948954774,-0.368339406993525,
9.51695131694362));
#24151=CARTESIAN_POINT('Ctrl Pts',(-1.62778015905473,-0.373313135664508,
9.1138728193103));
#24152=CARTESIAN_POINT('Ctrl Pts',(-1.50911575994275,-0.3758,8.94056871868047));
#24153=CARTESIAN_POINT('Ctrl Pts',(-1.72395594948115,-0.17793559721247,
9.64514957700335));
#24154=CARTESIAN_POINT('Ctrl Pts',(-1.71538533533075,-0.180422461547961,
9.43827577411898));
#24155=CARTESIAN_POINT('Ctrl Pts',(-1.59956980628701,-0.185396190218945,
9.02877619887675));
#24156=CARTESIAN_POINT('Ctrl Pts',(-1.16689349238722,-0.192856783225419,
8.55919520269185));
#24157=CARTESIAN_POINT('Ctrl Pts',(-0.56879336402393,-0.200317376231894,
8.33579973565633));
#24158=CARTESIAN_POINT('Ctrl Pts',(0.0657451987741329,-0.207777969238369,
8.40669336686818));
#24159=CARTESIAN_POINT('Ctrl Pts',(0.599793896721602,-0.215238562244844,
8.7566239434382));
#24160=CARTESIAN_POINT('Ctrl Pts',(0.918147075837748,-0.222699155251319,
9.31007624062289));
#24161=CARTESIAN_POINT('Ctrl Pts',(0.952115783961518,-0.230159748257794,
9.94765522057405));
#24162=CARTESIAN_POINT('Ctrl Pts',(0.694374175345971,-0.237620341264268,
10.531802683888));
#24163=CARTESIAN_POINT('Ctrl Pts',(0.200527242168716,-0.245080934270743,
10.9364941208908));
#24164=CARTESIAN_POINT('Ctrl Pts',(-0.422879800306456,-0.252541527277218,
11.0744187874602));
#24165=CARTESIAN_POINT('Ctrl Pts',(-1.04135074275375,-0.260002120283693,
10.9158206446354));
#24166=CARTESIAN_POINT('Ctrl Pts',(-1.52145391573408,-0.267462713290168,
10.4949161383219));
#24167=CARTESIAN_POINT('Ctrl Pts',(-1.75960988147327,-0.274923306296642,
9.90251307843778));
#24168=CARTESIAN_POINT('Ctrl Pts',(-1.70443783529711,-0.282383899303117,
9.26641897827667));
#24169=CARTESIAN_POINT('Ctrl Pts',(-1.36784084013167,-0.289844492309592,
8.72386748598803));
#24170=CARTESIAN_POINT('Ctrl Pts',(-0.8224377554211,-0.297305085316067,
8.39191097593678));
#24171=CARTESIAN_POINT('Ctrl Pts',(-0.185896155938985,-0.304765678322542,
8.34216710928376));
#24172=CARTESIAN_POINT('Ctrl Pts',(0.404453767748991,-0.312226271329017,
8.58536794226076));
#24173=CARTESIAN_POINT('Ctrl Pts',(0.821247432767259,-0.319686864335491,
9.06904406846149));
#24174=CARTESIAN_POINT('Ctrl Pts',(0.97456397482414,-0.327147457341966,
9.68884564197007));
#24175=CARTESIAN_POINT('Ctrl Pts',(0.831326302633348,-0.334608050348441,
10.3110529747565));
#24176=CARTESIAN_POINT('Ctrl Pts',(0.422436978585092,-0.342068643354916,
10.8014307367793));
#24177=CARTESIAN_POINT('Ctrl Pts',(-0.163888131079282,-0.349529236361391,
11.0541777598863));
#24178=CARTESIAN_POINT('Ctrl Pts',(-0.801153337032289,-0.356989829367866,
11.0147762690556));
#24179=CARTESIAN_POINT('Ctrl Pts',(-1.35187037119375,-0.36445042237434,
10.6917037649507));
#24180=CARTESIAN_POINT('Ctrl Pts',(-1.69722655295854,-0.371911015380815,
10.1547136291408));
#24181=CARTESIAN_POINT('Ctrl Pts',(-1.76269884616919,-0.37937160838729,
9.51955342619229));
#24182=CARTESIAN_POINT('Ctrl Pts',(-1.61032677969209,-0.384345337058273,
9.12220484843122));
#24183=CARTESIAN_POINT('Ctrl Pts',(-1.49334924183068,-0.386832201393765,
8.9513643339663));
#24184=CARTESIAN_POINT('Ctrl Pts',(-1.70486399362803,-0.188967798606235,
9.64594054127583));
#24185=CARTESIAN_POINT('Ctrl Pts',(-1.69641697104203,-0.191454662941727,
9.44204993848462));
#24186=CARTESIAN_POINT('Ctrl Pts',(-1.58227154663317,-0.19642839161271,
9.03845550518874));
#24187=CARTESIAN_POINT('Ctrl Pts',(-1.15583459219765,-0.203888984619185,
8.57564604823227));
#24188=CARTESIAN_POINT('Ctrl Pts',(-0.566359298558604,-0.211349577625659,
8.35547203006451));
#24189=CARTESIAN_POINT('Ctrl Pts',(0.0590289732250258,-0.218810170632134,
8.42534334774857));
#24190=CARTESIAN_POINT('Ctrl Pts',(0.585376482799404,-0.226270763638609,
8.77022779032738));
#24191=CARTESIAN_POINT('Ctrl Pts',(0.899138886184857,-0.233731356645084,
9.31569909174798));
#24192=CARTESIAN_POINT('Ctrl Pts',(0.932617752425185,-0.241191949651559,
9.94408393669573));
#24193=CARTESIAN_POINT('Ctrl Pts',(0.678592877296979,-0.248652542658033,
10.5198077681013));
#24194=CARTESIAN_POINT('Ctrl Pts',(0.191867407526504,-0.256113135664508,
10.9186633983672));
#24195=CARTESIAN_POINT('Ctrl Pts',(-0.422549864754182,-0.263573728670983,
11.0545991380042));
#24196=CARTESIAN_POINT('Ctrl Pts',(-1.03210221747478,-0.271034321677458,
10.8982880416196));
#24197=CARTESIAN_POINT('Ctrl Pts',(-1.50528211737561,-0.278494914683933,
10.4834531407609));
#24198=CARTESIAN_POINT('Ctrl Pts',(-1.74000378215801,-0.285955507690408,
9.89959276167443));
#24199=CARTESIAN_POINT('Ctrl Pts',(-1.68562733818473,-0.293416100696883,
9.27267138397698));
#24200=CARTESIAN_POINT('Ctrl Pts',(-1.35388420161973,-0.300876693703357,
8.73794369363799));
#24201=CARTESIAN_POINT('Ctrl Pts',(-0.816346039922294,-0.308337286709832,
8.41077412460057));
#24202=CARTESIAN_POINT('Ctrl Pts',(-0.188983616016791,-0.315797879716307,
8.36174758370636));
#24203=CARTESIAN_POINT('Ctrl Pts',(0.392853233890022,-0.323258472722782,
8.60144136679362));
#24204=CARTESIAN_POINT('Ctrl Pts',(0.803636573371775,-0.330719065729256,
9.07814269655022));
#24205=CARTESIAN_POINT('Ctrl Pts',(0.95474223171032,-0.338179658735732,
9.68900649211857));
#24206=CARTESIAN_POINT('Ctrl Pts',(0.81357010204384,-0.345640251742206,
10.3022413549873));
#24207=CARTESIAN_POINT('Ctrl Pts',(0.410577119884148,-0.353100844748681,
10.7855476803905));
#24208=CARTESIAN_POINT('Ctrl Pts',(-0.167292955370904,-0.360561437755156,
11.0346499938612));
#24209=CARTESIAN_POINT('Ctrl Pts',(-0.79536855106267,-0.368022030761631,
10.9958166877377));
#24210=CARTESIAN_POINT('Ctrl Pts',(-1.33814403300867,-0.375482623768106,
10.6774030138515));
#24211=CARTESIAN_POINT('Ctrl Pts',(-1.67852004532112,-0.38294321677458,
10.1481564830842));
#24212=CARTESIAN_POINT('Ctrl Pts',(-1.74304820279064,-0.390403809781055,
9.52215553544096));
#24213=CARTESIAN_POINT('Ctrl Pts',(-1.59287340032944,-0.395377538452038,
9.13053687755215));
#24214=CARTESIAN_POINT('Ctrl Pts',(-1.47758272371861,-0.39786440278753,
8.96215994925213));
#24215=CARTESIAN_POINT('Ctrl Pts',(-1.68577203777491,-0.2,9.64673150554831));
#24216=CARTESIAN_POINT('Ctrl Pts',(-1.67744860675331,-0.202486864335492,
9.44582410285027));
#24217=CARTESIAN_POINT('Ctrl Pts',(-1.56497328697934,-0.207460593006475,
9.04813481150073));
#24218=CARTESIAN_POINT('Ctrl Pts',(-1.14477569200808,-0.21492118601295,
8.59209689377269));
#24219=CARTESIAN_POINT('Ctrl Pts',(-0.563925233093278,-0.222381779019424,
8.3751443244727));
#24220=CARTESIAN_POINT('Ctrl Pts',(0.0523127476759186,-0.229842372025899,
8.44399332862896));
#24221=CARTESIAN_POINT('Ctrl Pts',(0.570959068877206,-0.237302965032374,
8.78383163721656));
#24222=CARTESIAN_POINT('Ctrl Pts',(0.880130696531965,-0.244763558038849,
9.32132194287307));
#24223=CARTESIAN_POINT('Ctrl Pts',(0.913119720888853,-0.252224151045324,
9.94051265281741));
#24224=CARTESIAN_POINT('Ctrl Pts',(0.662811579247987,-0.259684744051799,
10.5078128523146));
#24225=CARTESIAN_POINT('Ctrl Pts',(0.183207572884291,-0.267145337058273,
10.9008326758436));
#24226=CARTESIAN_POINT('Ctrl Pts',(-0.422219929201908,-0.274605930064748,
11.0347794885482));
#24227=CARTESIAN_POINT('Ctrl Pts',(-1.02285369219581,-0.282066523071223,
10.8807554386038));
#24228=CARTESIAN_POINT('Ctrl Pts',(-1.48911031901715,-0.289527116077698,
10.4719901431999));
#24229=CARTESIAN_POINT('Ctrl Pts',(-1.72039768284276,-0.296987709084173,
9.89667244491107));
#24230=CARTESIAN_POINT('Ctrl Pts',(-1.66681684107236,-0.304448302090648,
9.27892378967729));
#24231=CARTESIAN_POINT('Ctrl Pts',(-1.33992756310779,-0.311908895097122,
8.75201990128797));
#24232=CARTESIAN_POINT('Ctrl Pts',(-0.810254324423489,-0.319369488103597,
8.42963727326435));
#24233=CARTESIAN_POINT('Ctrl Pts',(-0.192071076094596,-0.326830081110072,
8.38132805812896));
#24234=CARTESIAN_POINT('Ctrl Pts',(0.381252700031053,-0.334290674116547,
8.61751479132649));
#24235=CARTESIAN_POINT('Ctrl Pts',(0.786025713976292,-0.341751267123022,
9.08724132463895));
#24236=CARTESIAN_POINT('Ctrl Pts',(0.934920488596498,-0.349211860129497,
9.68916734226706));
#24237=CARTESIAN_POINT('Ctrl Pts',(0.795813901454333,-0.356672453135971,
10.2934297352181));
#24238=CARTESIAN_POINT('Ctrl Pts',(0.398717261183206,-0.364133046142446,
10.7696646240018));
#24239=CARTESIAN_POINT('Ctrl Pts',(-0.170697779662527,-0.371593639148921,
11.0151222278361));
#24240=CARTESIAN_POINT('Ctrl Pts',(-0.789583765093051,-0.379054232155396,
10.9768571064198));
#24241=CARTESIAN_POINT('Ctrl Pts',(-1.3244176948236,-0.386514825161871,
10.6631022627523));
#24242=CARTESIAN_POINT('Ctrl Pts',(-1.6598135376837,-0.393975418168346,
10.1415993370275));
#24243=CARTESIAN_POINT('Ctrl Pts',(-1.7233975594121,-0.40143601117482,9.52475764468964));
#24244=CARTESIAN_POINT('Ctrl Pts',(-1.57542002096679,-0.406409739845804,
9.13886890667307));
#24245=CARTESIAN_POINT('Ctrl Pts',(-1.46181620560655,-0.408896604181295,
8.97295556453796));
#24246=CARTESIAN_POINT('',(-1.6839879813829,-0.2,9.6));
#24247=CARTESIAN_POINT('Ctrl Pts',(-1.74047515456274,-0.167429513866972,
9.6));
#24248=CARTESIAN_POINT('Ctrl Pts',(-1.73089506684943,-0.172953691659501,
9.6));
#24249=CARTESIAN_POINT('Ctrl Pts',(-1.72131152231067,-0.178479715438561,
9.6));
#24250=CARTESIAN_POINT('Ctrl Pts',(-1.70248475920816,-0.189335216828392,
9.6));
#24251=CARTESIAN_POINT('Ctrl Pts',(-1.69323488525986,-0.194668542692852,
9.6));
#24252=CARTESIAN_POINT('Ctrl Pts',(-1.6839879813829,-0.2,9.6));
#24253=CARTESIAN_POINT('',(-1.50911575994275,-0.3758,8.94056871868047));
#24254=CARTESIAN_POINT('Ctrl Pts',(-1.50911575994275,-0.3758,8.94056871868047));
#24255=CARTESIAN_POINT('Ctrl Pts',(-1.62778015905473,-0.373313135664508,
9.1138728193103));
#24256=CARTESIAN_POINT('Ctrl Pts',(-1.70506482430123,-0.370826271329017,
9.31541206812696));
#24257=CARTESIAN_POINT('Ctrl Pts',(-1.73263775209919,-0.368339406993525,
9.52356826891094));
#24258=CARTESIAN_POINT('Ctrl Pts',(-1.74038047358967,-0.367641073538499,
9.58202036732419));
#24259=CARTESIAN_POINT('Ctrl Pts',(-1.74420324577494,-0.366942740083473,
9.64099423620048));
#24260=CARTESIAN_POINT('Ctrl Pts',(-1.74415902867232,-0.366244406628447,
9.69997584025059));
#24261=CARTESIAN_POINT('Ctrl Pts',(-0.517805766168013,-0.3758,10.9813944679847));
#24262=CARTESIAN_POINT('Ctrl Pts',(-0.571473798863773,-0.3758,10.977632916352));
#24263=CARTESIAN_POINT('Ctrl Pts',(-0.624797035828109,-0.3758,10.9705481800708));
#24264=CARTESIAN_POINT('Ctrl Pts',(-0.677458301761716,-0.3758,10.9601736550514));
#24265=CARTESIAN_POINT('Ctrl Pts',(-0.711008440479028,-0.3758,10.9535641148636));
#24266=CARTESIAN_POINT('Ctrl Pts',(-0.744290045716627,-0.3758,10.9456182389887));
#24267=CARTESIAN_POINT('Ctrl Pts',(-0.777220103052431,-0.3758,10.9363336630147));
#24268=CARTESIAN_POINT('Ctrl Pts',(-0.799475508486024,-0.3758,10.9300587877397));
#24269=CARTESIAN_POINT('Ctrl Pts',(-0.821570315753372,-0.3758,10.9231722657496));
#24270=CARTESIAN_POINT('Ctrl Pts',(-0.843482780797905,-0.3758,10.9156861543558));
#24271=CARTESIAN_POINT('Ctrl Pts',(-0.855588446079938,-0.3758,10.9115504097642));
#24272=CARTESIAN_POINT('Ctrl Pts',(-0.867631229210224,-0.3758,10.9072340293321));
#24273=CARTESIAN_POINT('Ctrl Pts',(-0.87960107211078,-0.3758,10.9027421420255));
#24274=CARTESIAN_POINT('Ctrl Pts',(-0.930072327745337,-0.3758,10.8838019441952));
#24275=CARTESIAN_POINT('Ctrl Pts',(-0.979284885390671,-0.3758,10.8617328387111));
#24276=CARTESIAN_POINT('Ctrl Pts',(-1.02697484201776,-0.3758,10.8367178463095));
#24277=CARTESIAN_POINT('Ctrl Pts',(-1.05204499272848,-0.3758,10.8235677058211));
#24278=CARTESIAN_POINT('Ctrl Pts',(-1.07669414949484,-0.3758,10.8096026090408));
#24279=CARTESIAN_POINT('Ctrl Pts',(-1.10088170510615,-0.3758,10.794843848367));
#24280=CARTESIAN_POINT('Ctrl Pts',(-1.11352407473803,-0.3758,10.7871297283152));
#24281=CARTESIAN_POINT('Ctrl Pts',(-1.12604030512265,-0.3758,10.7791987260189));
#24282=CARTESIAN_POINT('Ctrl Pts',(-1.13842435602362,-0.3758,10.7710535225835));
#24283=CARTESIAN_POINT('Ctrl Pts',(-1.1482030472703,-0.3758,10.7646219090369));
#24284=CARTESIAN_POINT('Ctrl Pts',(-1.15790039230216,-0.3758,10.7580558360237));
#24285=CARTESIAN_POINT('Ctrl Pts',(-1.16749853219555,-0.3758,10.7513672969233));
#24286=CARTESIAN_POINT('Ctrl Pts',(-1.2120559830556,-0.3758,10.7203170876537));
#24287=CARTESIAN_POINT('Ctrl Pts',(-1.25455184393653,-0.3758,10.6865836476055));
#24288=CARTESIAN_POINT('Ctrl Pts',(-1.29472316146515,-0.3758,10.6503463122791));
#24289=CARTESIAN_POINT('Ctrl Pts',(-1.29783952021344,-0.3758,10.6475351389369));
#24290=CARTESIAN_POINT('Ctrl Pts',(-1.30094187788386,-0.3758,10.6447088735864));
#24291=CARTESIAN_POINT('Ctrl Pts',(-1.30403010538241,-0.3758,10.6418675885036));
#24292=CARTESIAN_POINT('Ctrl Pts',(-1.34319865735068,-0.3758,10.6058310521814));
#24293=CARTESIAN_POINT('Ctrl Pts',(-1.3800969660312,-0.3758,10.5673814429018));
#24294=CARTESIAN_POINT('Ctrl Pts',(-1.41457339153483,-0.3758,10.5267797716794));
#24295=CARTESIAN_POINT('Ctrl Pts',(-1.43911105221392,-0.3758,10.4978826335072));
#24296=CARTESIAN_POINT('Ctrl Pts',(-1.46242130487303,-0.3758,10.4678944751422));
#24297=CARTESIAN_POINT('Ctrl Pts',(-1.48443773672276,-0.3758,10.436899968734));
#24298=CARTESIAN_POINT('Ctrl Pts',(-1.49127119047245,-0.3758,10.4272799027996));
#24299=CARTESIAN_POINT('Ctrl Pts',(-1.4979799245099,-0.3758,10.417562843613));
#24300=CARTESIAN_POINT('Ctrl Pts',(-1.50456173213983,-0.3758,10.4077512091659));
#24301=CARTESIAN_POINT('Ctrl Pts',(-1.5106180016241,-0.3758,10.3987230051172));
#24302=CARTESIAN_POINT('Ctrl Pts',(-1.51656214228904,-0.3758,10.3896215694345));
#24303=CARTESIAN_POINT('Ctrl Pts',(-1.52238919234587,-0.3758,10.3804551888474));
#24304=CARTESIAN_POINT('Ctrl Pts',(-1.55171967266354,-0.3758,10.3343161746342));
#24305=CARTESIAN_POINT('Ctrl Pts',(-1.57811814740431,-0.3758,10.2864877234515));
#24306=CARTESIAN_POINT('Ctrl Pts',(-1.60143419434819,-0.3758,10.2372537515648));
#24307=CARTESIAN_POINT('Ctrl Pts',(-1.61710964099662,-0.3758,10.2041536080688));
#24308=CARTESIAN_POINT('Ctrl Pts',(-1.63139113760222,-0.3758,10.1704173283456));
#24309=CARTESIAN_POINT('Ctrl Pts',(-1.64422209280247,-0.3758,10.1361236501866));
#24310=CARTESIAN_POINT('Ctrl Pts',(-1.66233225904678,-0.3758,10.0877200665955));
#24311=CARTESIAN_POINT('Ctrl Pts',(-1.67755451722892,-0.3758,10.038206150238));
#24312=CARTESIAN_POINT('Ctrl Pts',(-1.68985348202901,-0.3758,9.98784757926546));
#24313=CARTESIAN_POINT('Ctrl Pts',(-1.69317156065143,-0.3758,9.97426158235309));
#24314=CARTESIAN_POINT('Ctrl Pts',(-1.69627663659562,-0.3758,9.96061406017673));
#24315=CARTESIAN_POINT('Ctrl Pts',(-1.69916749124626,-0.3758,9.94691015785263));
#24316=CARTESIAN_POINT('Ctrl Pts',(-1.70127082332291,-0.3758,9.93693945340117));
#24317=CARTESIAN_POINT('Ctrl Pts',(-1.70326097513578,-0.3758,9.9269372019356));
#24318=CARTESIAN_POINT('Ctrl Pts',(-1.70513458302098,-0.3758,9.91692190030026));
#24319=CARTESIAN_POINT('Ctrl Pts',(-1.71520308234393,-0.3758,9.86310110965825));
#24320=CARTESIAN_POINT('Ctrl Pts',(-1.72193246689098,-0.3758,9.80880465306829));
#24321=CARTESIAN_POINT('Ctrl Pts',(-1.72532846690209,-0.3758,9.75435546665585));
#24322=CARTESIAN_POINT('Ctrl Pts',(-1.72873261248714,-0.3758,9.69977567957408));
#24323=CARTESIAN_POINT('Ctrl Pts',(-1.72878752413501,-0.3758,9.64504135850294));
#24324=CARTESIAN_POINT('Ctrl Pts',(-1.72544849409975,-0.3758,9.59046698644781));
#24325=CARTESIAN_POINT('Ctrl Pts',(-1.72411676342687,-0.3758,9.5687006757372));
#24326=CARTESIAN_POINT('Ctrl Pts',(-1.7222445784162,-0.3758,9.54695977687243));
#24327=CARTESIAN_POINT('Ctrl Pts',(-1.71982677669824,-0.3758,9.52526435065811));
#24328=CARTESIAN_POINT('Ctrl Pts',(-1.71674242348629,-0.3758,9.49758782241691));
#24329=CARTESIAN_POINT('Ctrl Pts',(-1.7127702432767,-0.3758,9.46998524578407));
#24330=CARTESIAN_POINT('Ctrl Pts',(-1.70792192303047,-0.3758,9.44249519427747));
#24331=CARTESIAN_POINT('Ctrl Pts',(-1.70542336310974,-0.3758,9.42832832050983));
#24332=CARTESIAN_POINT('Ctrl Pts',(-1.70269065454176,-0.3758,9.41418548078457));
#24333=CARTESIAN_POINT('Ctrl Pts',(-1.69973255612478,-0.3758,9.4001052573882));
#24334=CARTESIAN_POINT('Ctrl Pts',(-1.68842261816779,-0.3758,9.3462711955736));
#24335=CARTESIAN_POINT('Ctrl Pts',(-1.67381149882828,-0.3758,9.29327608491672));
#24336=CARTESIAN_POINT('Ctrl Pts',(-1.65605749550781,-0.3758,9.24140245052763));
#24337=CARTESIAN_POINT('Ctrl Pts',(-1.63795749962153,-0.3758,9.1885178953036));
#24338=CARTESIAN_POINT('Ctrl Pts',(-1.61659072299859,-0.3758,9.13679785435062));
#24339=CARTESIAN_POINT('Ctrl Pts',(-1.5920708746144,-0.3758,9.08655183398384));
#24340=CARTESIAN_POINT('Ctrl Pts',(-1.56755102623021,-0.3758,9.03630581361707));
#24341=CARTESIAN_POINT('Ctrl Pts',(-1.53987774784311,-0.3758,8.98753269584568));
#24342=CARTESIAN_POINT('Ctrl Pts',(-1.50911575994275,-0.3758,8.94056871868047));
#24343=CARTESIAN_POINT('Ctrl Pts',(-1.6839753812096,-0.2,9.60000168607488));
#24344=CARTESIAN_POINT('Ctrl Pts',(-1.6848605948529,-0.2,9.61556437837414));
#24345=CARTESIAN_POINT('Ctrl Pts',(-1.68546042900379,-0.2,9.63114344455712));
#24346=CARTESIAN_POINT('Ctrl Pts',(-1.68577203777491,-0.2,9.64673150554831));
#24347=CARTESIAN_POINT('Ctrl Pts',(0.940308825950845,-0.117455697191997,
9.80220514213222));
#24348=CARTESIAN_POINT('Ctrl Pts',(0.928986682109438,-0.119218793569698,
9.95068269426644));
#24349=CARTESIAN_POINT('Ctrl Pts',(0.821349148298486,-0.1245080827028,10.3914498221302));
#24350=CARTESIAN_POINT('Ctrl Pts',(0.39736170109172,-0.131560468213604,
10.8545453758264));
#24351=CARTESIAN_POINT('Ctrl Pts',(-0.317535341911524,-0.140375950102109,
11.1001939757858));
#24352=CARTESIAN_POINT('Ctrl Pts',(-1.0932013213438,-0.149191431990614,
10.9720179261902));
#24353=CARTESIAN_POINT('Ctrl Pts',(-1.62266150701246,-0.158006913879118,
10.3886265975781));
#24354=CARTESIAN_POINT('Ctrl Pts',(-1.72939729330723,-0.163296203012221,
9.94849597778708));
#24355=CARTESIAN_POINT('Ctrl Pts',(-1.74047515456274,-0.165059299389922,
9.8));
#24356=CARTESIAN_POINT('Ctrl Pts',(0.921255807191823,-0.128487898585762,
9.80075225571335));
#24357=CARTESIAN_POINT('Ctrl Pts',(0.910094612092099,-0.130250994963463,
9.94711914086446));
#24358=CARTESIAN_POINT('Ctrl Pts',(0.803987188290995,-0.135540284096565,
10.3816205901078));
#24359=CARTESIAN_POINT('Ctrl Pts',(0.386026889923967,-0.142592669607369,
10.838133057801));
#24360=CARTESIAN_POINT('Ctrl Pts',(-0.318707609561407,-0.151408151495874,
11.0802896659951));
#24361=CARTESIAN_POINT('Ctrl Pts',(-1.08334719106904,-0.160223633384379,
10.9539356895144));
#24362=CARTESIAN_POINT('Ctrl Pts',(-1.60528089130808,-0.169039115272883,
10.3788374988066));
#24363=CARTESIAN_POINT('Ctrl Pts',(-1.71049938628971,-0.174328404405986,
9.94496350942258));
#24364=CARTESIAN_POINT('Ctrl Pts',(-1.72141977137688,-0.176091500783687,
9.79857846054655));
#24365=CARTESIAN_POINT('Ctrl Pts',(0.902202788432801,-0.139520099979527,
9.79929936929449));
#24366=CARTESIAN_POINT('Ctrl Pts',(0.891202542074759,-0.141283196357228,
9.94355558746248));
#24367=CARTESIAN_POINT('Ctrl Pts',(0.786625228283503,-0.146572485490331,
10.3717913580854));
#24368=CARTESIAN_POINT('Ctrl Pts',(0.374692078756213,-0.153624871001134,
10.8217207397756));
#24369=CARTESIAN_POINT('Ctrl Pts',(-0.319879877211292,-0.162440352889639,
11.0603853562044));
#24370=CARTESIAN_POINT('Ctrl Pts',(-1.07349306079427,-0.171255834778144,
10.9358534528386));
#24371=CARTESIAN_POINT('Ctrl Pts',(-1.5879002756037,-0.180071316666648,
10.369048400035));
#24372=CARTESIAN_POINT('Ctrl Pts',(-1.69160147927219,-0.185360605799751,
9.9414310410581));
#24373=CARTESIAN_POINT('Ctrl Pts',(-1.70236438819101,-0.187123702177452,
9.79715692109309));
#24374=CARTESIAN_POINT('Ctrl Pts',(0.883149769673779,-0.150552301373292,
9.79784648287562));
#24375=CARTESIAN_POINT('Ctrl Pts',(0.87231047205742,-0.152315397750993,
9.9399920340605));
#24376=CARTESIAN_POINT('Ctrl Pts',(0.769263268276011,-0.157604686884096,
10.361962126063));
#24377=CARTESIAN_POINT('Ctrl Pts',(0.36335726758846,-0.164657072394899,
10.8053084217502));
#24378=CARTESIAN_POINT('Ctrl Pts',(-0.321052144861175,-0.173472554283404,
11.0404810464137));
#24379=CARTESIAN_POINT('Ctrl Pts',(-1.0636389305195,-0.182288036171909,
10.9177712161628));
#24380=CARTESIAN_POINT('Ctrl Pts',(-1.57051965989932,-0.191103518060414,
10.3592593012635));
#24381=CARTESIAN_POINT('Ctrl Pts',(-1.67270357225468,-0.196392807193516,
9.9378985726936));
#24382=CARTESIAN_POINT('Ctrl Pts',(-1.68330900500515,-0.198155903571217,
9.79573538163964));
#24383=CARTESIAN_POINT('',(0.882983735526293,-0.150579014154542,9.8));
#24384=CARTESIAN_POINT('Ctrl Pts',(0.911390797333273,-0.134200000000245,
9.80000000017706));
#24385=CARTESIAN_POINT('Ctrl Pts',(0.901922957108531,-0.139659147854633,
9.80000000017706));
#24386=CARTESIAN_POINT('Ctrl Pts',(0.892451669119078,-0.145120130049362,
9.8));
#24387=CARTESIAN_POINT('Ctrl Pts',(0.882983735526293,-0.150579014154542,
9.8));
#24388=CARTESIAN_POINT('',(-1.74047515456274,-0.165059299389922,9.8));
#24389=CARTESIAN_POINT('Ctrl Pts',(-1.74047515456274,-0.165059299389922,
9.8));
#24390=CARTESIAN_POINT('Ctrl Pts',(-1.72939729330723,-0.163296203012221,
9.94849597778708));
#24391=CARTESIAN_POINT('Ctrl Pts',(-1.69381869787564,-0.16153310663452,
10.0952061843841));
#24392=CARTESIAN_POINT('Ctrl Pts',(-1.63480228854334,-0.15977001025682,
10.2319057440229));
#24393=CARTESIAN_POINT('Ctrl Pts',(-1.51676946987873,-0.156243817501418,
10.5053048633005));
#24394=CARTESIAN_POINT('Ctrl Pts',(-1.30498539561127,-0.152717624746016,
10.7386613947454));
#24395=CARTESIAN_POINT('Ctrl Pts',(-1.04396016259108,-0.149191431990614,
10.8809748703869));
#24396=CARTESIAN_POINT('Ctrl Pts',(-0.782934929570892,-0.145665239235212,
11.0232883460284));
#24397=CARTESIAN_POINT('Ctrl Pts',(-0.472668537797981,-0.14213904647981,
11.0745587658667));
#24398=CARTESIAN_POINT('Ctrl Pts',(-0.17860719573948,-0.138612853724408,
11.0261426124902));
#24399=CARTESIAN_POINT('Ctrl Pts',(-0.0559395124477826,-0.13714190248302,
11.0059458150227));
#24400=CARTESIAN_POINT('Ctrl Pts',(0.0639082635928698,-0.135670951241633,
10.9684021475613));
#24401=CARTESIAN_POINT('Ctrl Pts',(0.176129947875697,-0.134200000000245,
10.9150835725709));
#24402=CARTESIAN_POINT('',(-1.68298373552629,-0.198103007464943,9.8));
#24403=CARTESIAN_POINT('Ctrl Pts',(-1.68298373552629,-0.198103007464943,
9.8));
#24404=CARTESIAN_POINT('Ctrl Pts',(-1.69256533649058,-0.192597003527467,
9.8));
#24405=CARTESIAN_POINT('Ctrl Pts',(-1.70215018540065,-0.187088555034124,
9.8));
#24406=CARTESIAN_POINT('Ctrl Pts',(-1.72131168622614,-0.176075287080509,
9.8));
#24407=CARTESIAN_POINT('Ctrl Pts',(-1.73089522164625,-0.170566511327364,
9.8));
#24408=CARTESIAN_POINT('Ctrl Pts',(-1.74047515456274,-0.165059299389922,
9.8));
#24409=CARTESIAN_POINT('Ctrl Pts',(0.882983744031739,-0.150579014154542,
9.80000002381835));
#24410=CARTESIAN_POINT('Ctrl Pts',(0.871962951449779,-0.152333206271826,
9.94141251268902));
#24411=CARTESIAN_POINT('Ctrl Pts',(0.768750776052023,-0.157613591144512,
10.3625218899706));
#24412=CARTESIAN_POINT('Ctrl Pts',(0.36335726758846,-0.164657072394899,
10.8053084217502));
#24413=CARTESIAN_POINT('Ctrl Pts',(-0.321052144861175,-0.173472554283404,
11.0404810464137));
#24414=CARTESIAN_POINT('Ctrl Pts',(-1.0636389305195,-0.182288036171909,
10.9177712161628));
#24415=CARTESIAN_POINT('Ctrl Pts',(-1.56950583682196,-0.191085886024989,
10.3603763929884));
#24416=CARTESIAN_POINT('Ctrl Pts',(-1.67202006066509,-0.196357543122667,
9.94070685646919));
#24417=CARTESIAN_POINT('Ctrl Pts',(-1.68298378608493,-0.198103007464943,
9.80000001577842));
#24418=CARTESIAN_POINT('Ctrl Pts',(0.361156509406693,-0.120274170443804,
8.63259693702807));
#24419=CARTESIAN_POINT('Ctrl Pts',(0.494579708156992,-0.122263574666153,
8.72773994322471));
#24420=CARTESIAN_POINT('Ctrl Pts',(0.763931929792523,-0.126905517851633,
9.00874498271484));
#24421=CARTESIAN_POINT('Ctrl Pts',(0.890509390304728,-0.131547461037113,
9.38214093563506));
#24422=CARTESIAN_POINT('Ctrl Pts',(0.907175784144597,-0.134200000000245,
9.6));
#24423=CARTESIAN_POINT('Ctrl Pts',(0.35648848307094,-0.124916113629284,
8.63914311451882));
#24424=CARTESIAN_POINT('Ctrl Pts',(0.48909342302969,-0.126905517851633,
8.73370262697521));
#24425=CARTESIAN_POINT('Ctrl Pts',(0.75679375934512,-0.131547461037113,
9.01298431665672));
#24426=CARTESIAN_POINT('Ctrl Pts',(0.882594944660462,-0.136189404222593,
9.38409030408318));
#24427=CARTESIAN_POINT('Ctrl Pts',(0.899159126715494,-0.138841943185725,
9.60061328074819));
#24428=CARTESIAN_POINT('Ctrl Pts',(0.351820456735188,-0.129558056814764,
8.64568929200957));
#24429=CARTESIAN_POINT('Ctrl Pts',(0.483607137902389,-0.131547461037113,
8.73966531072571));
#24430=CARTESIAN_POINT('Ctrl Pts',(0.749655588897719,-0.136189404222593,
9.0172236505986));
#24431=CARTESIAN_POINT('Ctrl Pts',(0.874680499016197,-0.140831347408073,
9.38603967253129));
#24432=CARTESIAN_POINT('Ctrl Pts',(0.891142469286392,-0.143483886371205,
9.60122656149638));
#24433=CARTESIAN_POINT('Ctrl Pts',(0.347152430399435,-0.134200000000245,
8.65223546950032));
#24434=CARTESIAN_POINT('Ctrl Pts',(0.478120852775088,-0.136189404222593,
8.74562799447621));
#24435=CARTESIAN_POINT('Ctrl Pts',(0.742517418450316,-0.140831347408073,
9.02146298454048));
#24436=CARTESIAN_POINT('Ctrl Pts',(0.866766053371931,-0.145473290593554,
9.3879890409794));
#24437=CARTESIAN_POINT('Ctrl Pts',(0.883125811857289,-0.148125829556685,
9.60183984224456));
#24438=CARTESIAN_POINT('',(0.882983735526293,-0.148103007464943,9.6));
#24439=CARTESIAN_POINT('Ctrl Pts',(0.882983735526293,-0.148103007464943,
9.6));
#24440=CARTESIAN_POINT('Ctrl Pts',(0.891046845655766,-0.143469594292482,
9.6));
#24441=CARTESIAN_POINT('Ctrl Pts',(0.899112255838064,-0.138834449992759,
9.6));
#24442=CARTESIAN_POINT('Ctrl Pts',(0.907175784144596,-0.134200000000245,
9.6));
#24443=CARTESIAN_POINT('Ctrl Pts',(0.347152430399435,-0.134200000000245,
8.65223546950032));
#24444=CARTESIAN_POINT('Ctrl Pts',(0.478120852775088,-0.136189404222593,
8.74562799447621));
#24445=CARTESIAN_POINT('Ctrl Pts',(0.742084116961616,-0.140823740044159,
9.02101093739862));
#24446=CARTESIAN_POINT('Ctrl Pts',(0.866358431749138,-0.145458075865725,
9.38678793547139));
#24447=CARTESIAN_POINT('Ctrl Pts',(0.882983706628455,-0.148103007464943,
9.60000000779774));
#24448=CARTESIAN_POINT('Origin',(-0.4,0.0506589891902575,9.7));
#24449=CARTESIAN_POINT('',(0.882983735526293,0.0506589891902575,9.8));
#24450=CARTESIAN_POINT('',(-1.68298373552629,-0.2,9.8));
#24451=CARTESIAN_POINT('',(-1.68298373552629,0.0506589891902575,9.8));
#24452=CARTESIAN_POINT('Origin',(-0.4,-0.2,9.7));
#24453=CARTESIAN_POINT('Origin',(-0.4,0.0506589891902575,9.7));
#24454=CARTESIAN_POINT('',(0.882983735526293,0.0506589891902575,9.6));
#24455=CARTESIAN_POINT('Origin',(-0.4,-0.3758,9.7));
#24456=CARTESIAN_POINT('',(-1.7442,-0.375799999999999,9.7));
#24457=CARTESIAN_POINT('Origin',(-0.4,-0.3758,9.7));
#24458=CARTESIAN_POINT('Origin',(-0.4,-0.3758,9.7));
#24459=CARTESIAN_POINT('Ctrl Pts',(-0.963302249831946,-0.117455697189843,
10.888459674838));
#24460=CARTESIAN_POINT('Ctrl Pts',(-1.17201968067454,-0.120250778212055,
10.7895324660635));
#24461=CARTESIAN_POINT('Ctrl Pts',(-1.5358329245996,-0.125840940256479,
10.4792728901217));
#24462=CARTESIAN_POINT('Ctrl Pts',(-1.69437043704508,-0.131431102300903,
10.0281776251649));
#24463=CARTESIAN_POINT('Ctrl Pts',(-1.71155353730395,-0.134226183323115,
9.79784243541102));
#24464=CARTESIAN_POINT('Ctrl Pts',(-0.967442787905632,-0.123037131459977,
10.8971954157908));
#24465=CARTESIAN_POINT('Ctrl Pts',(-1.17769439062363,-0.125832212482189,
10.7975410452225));
#24466=CARTESIAN_POINT('Ctrl Pts',(-1.54418183403686,-0.131422374526613,
10.4850009145922));
#24467=CARTESIAN_POINT('Ctrl Pts',(-1.70388467221392,-0.137012536571037,
10.0305898859935));
#24468=CARTESIAN_POINT('Ctrl Pts',(-1.72119407639022,-0.139807617593249,
9.79856162360734));
#24469=CARTESIAN_POINT('Ctrl Pts',(-0.971583325979318,-0.128618565730111,
10.9059311567437));
#24470=CARTESIAN_POINT('Ctrl Pts',(-1.18336910057272,-0.131413646752323,
10.8055496243816));
#24471=CARTESIAN_POINT('Ctrl Pts',(-1.55253074347412,-0.137003808796747,
10.4907289390627));
#24472=CARTESIAN_POINT('Ctrl Pts',(-1.71339890738276,-0.142593970841171,
10.033002146822));
#24473=CARTESIAN_POINT('Ctrl Pts',(-1.73083461547648,-0.145389051863383,
9.79928081180367));
#24474=CARTESIAN_POINT('Ctrl Pts',(-0.975723864053004,-0.134200000000245,
10.9146668976966));
#24475=CARTESIAN_POINT('Ctrl Pts',(-1.18904381052181,-0.136995081022457,
10.8135582035406));
#24476=CARTESIAN_POINT('Ctrl Pts',(-1.56087965291138,-0.142585243066881,
10.4964569635332));
#24477=CARTESIAN_POINT('Ctrl Pts',(-1.7229131425516,-0.148175405111305,
10.0354144076506));
#24478=CARTESIAN_POINT('Ctrl Pts',(-1.74047515456274,-0.150970486133517,
9.79999999999999));
#24479=CARTESIAN_POINT('',(-1.74047515456274,-0.150970486133517,9.8));
#24480=CARTESIAN_POINT('Ctrl Pts',(-1.74047515456274,-0.150970486133517,
9.8));
#24481=CARTESIAN_POINT('Ctrl Pts',(-1.73089506685314,-0.145446308343123,
9.8));
#24482=CARTESIAN_POINT('Ctrl Pts',(-1.72131152231243,-0.139920284562941,
9.8));
#24483=CARTESIAN_POINT('Ctrl Pts',(-1.7116177775445,-0.134330876589416,
9.8));
#24484=CARTESIAN_POINT('Ctrl Pts',(-1.71150428769636,-0.134265438426614,
9.8));
#24485=CARTESIAN_POINT('Ctrl Pts',(-1.71139079735282,-0.134200000000245,
9.8));
#24486=CARTESIAN_POINT('Ctrl Pts',(-0.975723864053004,-0.134200000000245,
10.9146668976966));
#24487=CARTESIAN_POINT('Ctrl Pts',(-1.18904381052181,-0.136995081022457,
10.8135582035406));
#24488=CARTESIAN_POINT('Ctrl Pts',(-1.3749617317166,-0.139790162044669,
10.6550075835369));
#24489=CARTESIAN_POINT('Ctrl Pts',(-1.50842906472404,-0.142585243066881,
10.4604716345644));
#24490=CARTESIAN_POINT('Ctrl Pts',(-1.64189639773149,-0.145380324089093,
10.2659356855919));
#24491=CARTESIAN_POINT('Ctrl Pts',(-1.7229131425516,-0.148175405111305,
10.0354144076506));
#24492=CARTESIAN_POINT('Ctrl Pts',(-1.74047515456274,-0.150970486133517,
9.79999999999999));
#24493=CARTESIAN_POINT('Origin',(0.6,-0.1,9.6));
#24494=CARTESIAN_POINT('',(0.906177629574171,-0.1,9.6));
#24495=CARTESIAN_POINT('Ctrl Pts',(0.906177629574171,-0.1,9.6));
#24496=CARTESIAN_POINT('Ctrl Pts',(0.923105426092673,-0.116878403916367,
9.6));
#24497=CARTESIAN_POINT('Ctrl Pts',(0.940475154562984,-0.134200000000245,
9.6));
#24498=CARTESIAN_POINT('',(0.675360404701605,-0.1,9.6));
#24499=CARTESIAN_POINT('',(0.755,-0.1,9.6));
#24500=CARTESIAN_POINT('',(0.645227248018344,-0.13,9.6));
#24501=CARTESIAN_POINT('Ctrl Pts',(0.645227248018343,-0.13,9.6));
#24502=CARTESIAN_POINT('Ctrl Pts',(0.660081620885339,-0.115213147359248,
9.6));
#24503=CARTESIAN_POINT('Ctrl Pts',(0.675360404701605,-0.1,9.6));
#24504=CARTESIAN_POINT('',(0.645227248018344,-0.2,9.6));
#24505=CARTESIAN_POINT('',(0.645227248018344,-0.265,9.6));
#24506=CARTESIAN_POINT('',(0.6,-0.2,9.6));
#24507=CARTESIAN_POINT('Origin',(-1.8,-0.1,9.6));
#24508=CARTESIAN_POINT('',(-1.44522724801834,-0.2,9.6));
#24509=CARTESIAN_POINT('',(-1.4,-0.2,9.6));
#24510=CARTESIAN_POINT('',(-1.44522724801834,-0.13,9.6));
#24511=CARTESIAN_POINT('',(-1.44522724801834,-0.265,9.6));
#24512=CARTESIAN_POINT('',(-1.4753604047016,-0.1,9.6));
#24513=CARTESIAN_POINT('Ctrl Pts',(-1.4753604047016,-0.1,9.6));
#24514=CARTESIAN_POINT('Ctrl Pts',(-1.46008162088557,-0.11521314735902,
9.6));
#24515=CARTESIAN_POINT('Ctrl Pts',(-1.44522724801834,-0.13,9.6));
#24516=CARTESIAN_POINT('',(-1.70617762957417,-0.1,9.6));
#24517=CARTESIAN_POINT('',(-0.445,-0.1,9.6));
#24518=CARTESIAN_POINT('Ctrl Pts',(-1.74047515456298,-0.134200000000245,
9.6));
#24519=CARTESIAN_POINT('Ctrl Pts',(-1.72310542608936,-0.116878403913059,
9.6));
#24520=CARTESIAN_POINT('Ctrl Pts',(-1.70617762957417,-0.1,9.6));
#24521=CARTESIAN_POINT('Origin',(-0.4,-0.255,9.7));
#24522=CARTESIAN_POINT('Origin',(-0.4,-0.3758,9.7));
#24523=CARTESIAN_POINT('Origin',(-0.4,-0.255,9.7));
#24524=CARTESIAN_POINT('',(-1.74047515456274,-0.255,9.8));
#24525=CARTESIAN_POINT('Origin',(-0.4,-0.1342,9.7));
#24526=CARTESIAN_POINT('Origin',(-1.6,-0.2,9.7));
#24527=CARTESIAN_POINT('',(-1.44522724801834,-0.2,9.8));
#24528=CARTESIAN_POINT('',(-1.8,-0.2,9.8));
#24529=CARTESIAN_POINT('',(-1.45,-0.2,9.7));
#24530=CARTESIAN_POINT('Origin',(-0.4,-0.2,9.7));
#24531=CARTESIAN_POINT('Origin',(-0.4,-0.2,9.7));
#24532=CARTESIAN_POINT('Origin',(-1.4,-0.1,9.8));
#24533=CARTESIAN_POINT('',(-1.70617762957417,-0.1,9.8));
#24534=CARTESIAN_POINT('Ctrl Pts',(-1.70617762957417,-0.1,9.8));
#24535=CARTESIAN_POINT('Ctrl Pts',(-1.72310542608936,-0.116878403913059,
9.8));
#24536=CARTESIAN_POINT('Ctrl Pts',(-1.74047515456298,-0.134200000000246,
9.8));
#24537=CARTESIAN_POINT('',(-1.4753604047016,-0.1,9.8));
#24538=CARTESIAN_POINT('',(-0.245,-0.1,9.8));
#24539=CARTESIAN_POINT('',(-1.44522724801834,-0.13,9.8));
#24540=CARTESIAN_POINT('Ctrl Pts',(-1.44522724801834,-0.13,9.8));
#24541=CARTESIAN_POINT('Ctrl Pts',(-1.46008162088557,-0.11521314735902,
9.8));
#24542=CARTESIAN_POINT('Ctrl Pts',(-1.4753604047016,-0.1,9.8));
#24543=CARTESIAN_POINT('',(-1.44522724801834,-0.265,9.8));
#24544=CARTESIAN_POINT('Origin',(0.8,-0.2,9.7));
#24545=CARTESIAN_POINT('',(0.645227248018344,-0.2,9.8));
#24546=CARTESIAN_POINT('Origin',(-0.4,-0.2,9.7));
#24547=CARTESIAN_POINT('',(1.,-0.2,9.8));
#24548=CARTESIAN_POINT('Origin',(1.,-0.1,9.8));
#24549=CARTESIAN_POINT('',(0.645227248018344,-0.13,9.8));
#24550=CARTESIAN_POINT('',(0.645227248018344,-0.265,9.8));
#24551=CARTESIAN_POINT('',(0.675360404701605,-0.1,9.8));
#24552=CARTESIAN_POINT('Ctrl Pts',(0.675360404701605,-0.1,9.8));
#24553=CARTESIAN_POINT('Ctrl Pts',(0.660081620885339,-0.115213147359248,
9.8));
#24554=CARTESIAN_POINT('Ctrl Pts',(0.645227248018343,-0.13,9.8));
#24555=CARTESIAN_POINT('',(0.906177629574171,-0.1,9.8));
#24556=CARTESIAN_POINT('',(0.955,-0.1,9.8));
#24557=CARTESIAN_POINT('Ctrl Pts',(0.940475154562984,-0.134200000000246,
9.80000000000001));
#24558=CARTESIAN_POINT('Ctrl Pts',(0.923105426092674,-0.116878403916367,
9.8));
#24559=CARTESIAN_POINT('Ctrl Pts',(0.906177629574171,-0.1,9.8));
#24560=CARTESIAN_POINT('Origin',(-0.4,-0.265,9.7));
#24561=CARTESIAN_POINT('',(-1.45,-0.4,9.7));
#24562=CARTESIAN_POINT('Origin',(-0.4,-0.4,9.7));
#24563=CARTESIAN_POINT('',(-1.45,-0.265,9.7));
#24564=CARTESIAN_POINT('Origin',(-0.4,-0.13,9.7));
#24565=CARTESIAN_POINT('Origin',(-0.4,-0.13,9.7));
#24566=CARTESIAN_POINT('Origin',(-0.4,-0.12,9.7));
#24567=CARTESIAN_POINT('Origin',(-0.4,-0.1,9.7));
#24568=CARTESIAN_POINT('Origin',(-0.4,-0.12,9.7));
#24569=CARTESIAN_POINT('Origin',(-0.4,-0.1,9.7));
#24570=CARTESIAN_POINT('Origin',(0.91,-0.1,9.7));
#24571=CARTESIAN_POINT('Origin',(-0.4,-0.1,9.7));
#24572=CARTESIAN_POINT('Origin',(0.91,-0.1,9.7));
#24573=CARTESIAN_POINT('Origin',(-0.4,-0.1,9.7));
#24574=CARTESIAN_POINT('Origin',(-0.4,-0.115,9.7));
#24575=CARTESIAN_POINT('Origin',(-0.4,-0.115,9.7));
#24576=CARTESIAN_POINT('Origin',(-0.4,-0.385,9.7));
#24577=CARTESIAN_POINT('',(-1.72,-0.4,9.7));
#24578=CARTESIAN_POINT('Origin',(-0.4,-0.4,9.7));
#24579=CARTESIAN_POINT('',(-1.735,-0.385,9.7));
#24580=CARTESIAN_POINT('Origin',(0.65,-0.4,9.7));
#24581=CARTESIAN_POINT('',(0.,0.,0.));
#24582=CARTESIAN_POINT('Origin',(0.,0.,-0.24));
#24583=CARTESIAN_POINT('',(-0.195553227933509,0.000153074281780883,-0.430479697454243));
#24584=CARTESIAN_POINT('',(-0.195558160953945,0.000205798840386435,-0.44065363587909));
#24585=CARTESIAN_POINT('',(-0.1954,-2.39295984553393E-17,-0.24));
#24586=CARTESIAN_POINT('',(0.0862535085070011,0.17548972741326,-0.453066666666667));
#24587=CARTESIAN_POINT('Ctrl Pts',(-0.195553227933509,0.000153074281780883,
-0.430479697454243));
#24588=CARTESIAN_POINT('Ctrl Pts',(-0.195630430217605,0.00963779447124953,
-0.43102175579123));
#24589=CARTESIAN_POINT('Ctrl Pts',(-0.194998712214993,0.019111688516455,
-0.431563814128216));
#24590=CARTESIAN_POINT('Ctrl Pts',(-0.193622187496123,0.0284754106320751,
-0.432105872465203));
#24591=CARTESIAN_POINT('Ctrl Pts',(-0.184317635852011,0.091769033195883,
-0.435769889334259));
#24592=CARTESIAN_POINT('Ctrl Pts',(-0.140982731022398,0.150028880428339,
-0.439433906203315));
#24593=CARTESIAN_POINT('Ctrl Pts',(-0.0830410591985528,0.177195443378647,
-0.443097923072371));
#24594=CARTESIAN_POINT('Ctrl Pts',(-0.0304934781803096,0.201832930055914,
-0.446420837603803));
#24595=CARTESIAN_POINT('Ctrl Pts',(0.0340678230776199,0.200896926114329,
-0.449743752135234));
#24596=CARTESIAN_POINT('Ctrl Pts',(0.0863544310469484,0.175597323663767,
-0.453066666666667));
#24597=CARTESIAN_POINT('',(-0.0861525859670531,0.175382131162754,-0.453066666666667));
#24598=CARTESIAN_POINT('Origin',(0.,0.,-0.453066666666667));
#24599=CARTESIAN_POINT('Ctrl Pts',(-0.0861525859670524,0.175382131162755,
-0.453066666666667));
#24600=CARTESIAN_POINT('Ctrl Pts',(-0.143832504185423,0.147048149360074,
-0.449402649797611));
#24601=CARTESIAN_POINT('Ctrl Pts',(-0.185985128745257,0.0883085765373875,
-0.445738632928555));
#24602=CARTESIAN_POINT('Ctrl Pts',(-0.194094856498636,0.0249448584907909,
-0.442074616059499));
#24603=CARTESIAN_POINT('Ctrl Pts',(-0.195143228892278,0.0167536127697661,
-0.441600955999363));
#24604=CARTESIAN_POINT('Ctrl Pts',(-0.195622689264249,0.00848509008189603,
-0.441127295939226));
#24605=CARTESIAN_POINT('Ctrl Pts',(-0.195558160953945,0.000205798840386435,
-0.44065363587909));
#24606=CARTESIAN_POINT('Origin',(0.,0.,-0.24));
#24607=CARTESIAN_POINT('',(-0.195096259697753,-1.61683889792347E-5,-0.360479697454244));
#24608=CARTESIAN_POINT('',(-0.1950945860993,3.61475788830789E-6,-0.37065363587909));
#24609=CARTESIAN_POINT('',(-0.1954,-2.39295984553393E-17,-0.24));
#24610=CARTESIAN_POINT('Ctrl Pts',(-0.195096259697753,-1.61683889792347E-5,
-0.360479697454244));
#24611=CARTESIAN_POINT('Ctrl Pts',(-0.195070888875686,0.0332768877299866,
-0.362370987910228));
#24612=CARTESIAN_POINT('Ctrl Pts',(-0.186971229054641,0.0665814795668455,
-0.364262278366212));
#24613=CARTESIAN_POINT('Ctrl Pts',(-0.170868833427777,0.0954169932588536,
-0.366153568822197));
#24614=CARTESIAN_POINT('Ctrl Pts',(-0.139673493218476,0.151280336861681,
-0.369817585691253));
#24615=CARTESIAN_POINT('Ctrl Pts',(-0.078442509106134,0.190370461531553,
-0.373481602560308));
#24616=CARTESIAN_POINT('Ctrl Pts',(-0.0146381891088212,0.195156588972792,
-0.377145619429364));
#24617=CARTESIAN_POINT('Ctrl Pts',(0.0491661308884916,0.199942716414032,
-0.38080963629842));
#24618=CARTESIAN_POINT('Ctrl Pts',(0.115543786770775,0.17042484662664,-0.384473653167476));
#24619=CARTESIAN_POINT('Ctrl Pts',(0.154723399880928,0.119839217267535,
-0.388137670036532));
#24620=CARTESIAN_POINT('Ctrl Pts',(0.193903012991081,0.0692535879084296,
-0.391801686905588));
#24621=CARTESIAN_POINT('Ctrl Pts',(0.205884583329105,-0.00239980102238897,
-0.395465703774644));
#24622=CARTESIAN_POINT('Ctrl Pts',(0.185295223086548,-0.062978599706434,
-0.3991297206437));
#24623=CARTESIAN_POINT('Ctrl Pts',(0.16470586284399,-0.123557398390479,
-0.402793737512756));
#24624=CARTESIAN_POINT('Ctrl Pts',(0.111545572020852,-0.173061606827751,
-0.406457754381811));
#24625=CARTESIAN_POINT('Ctrl Pts',(0.0496553570667544,-0.189298243122558,
-0.410121771250867));
#24626=CARTESIAN_POINT('Ctrl Pts',(-0.012234857887343,-0.205534879417366,
-0.413785788119923));
#24627=CARTESIAN_POINT('Ctrl Pts',(-0.0828549969723998,-0.188503943569709,
-0.417449804988979));
#24628=CARTESIAN_POINT('Ctrl Pts',(-0.130527967285623,-0.145824776698301,
-0.421113821858035));
#24629=CARTESIAN_POINT('Ctrl Pts',(-0.171148150471846,-0.109459608655245,
-0.424235780390105));
#24630=CARTESIAN_POINT('Ctrl Pts',(-0.195108585146772,-0.0544737086663899,
-0.427357738922174));
#24631=CARTESIAN_POINT('Ctrl Pts',(-0.195553227933509,0.000153074281780883,
-0.430479697454243));
#24632=CARTESIAN_POINT('Ctrl Pts',(-0.195558160953945,0.000205798840386435,
-0.44065363587909));
#24633=CARTESIAN_POINT('Ctrl Pts',(-0.1951235278669,-0.0555597077082796,
-0.437463279070171));
#24634=CARTESIAN_POINT('Ctrl Pts',(-0.170009480570289,-0.111813756765947,
-0.434272922261251));
#24635=CARTESIAN_POINT('Ctrl Pts',(-0.12783196242833,-0.14823305616899,
-0.431082565452331));
#24636=CARTESIAN_POINT('Ctrl Pts',(-0.0793925096577201,-0.190059389511667,
-0.427418548583275));
#24637=CARTESIAN_POINT('Ctrl Pts',(-0.00844677316957623,-0.205724192926515,
-0.42375453171422));
#24638=CARTESIAN_POINT('Ctrl Pts',(0.0531396320705838,-0.188335328572067,
-0.420090514845164));
#24639=CARTESIAN_POINT('Ctrl Pts',(0.114726037310744,-0.170946464217619,
-0.416426497976108));
#24640=CARTESIAN_POINT('Ctrl Pts',(0.16695311130292,-0.120503932093875,
-0.412762481107052));
#24641=CARTESIAN_POINT('Ctrl Pts',(0.186420314612119,-0.0595639392003285,
-0.409098464237996));
#24642=CARTESIAN_POINT('Ctrl Pts',(0.205887517921318,0.00137605369321816,
-0.40543444736894));
#24643=CARTESIAN_POINT('Ctrl Pts',(0.192594850547539,0.0728135073565672,
-0.401770430499884));
#24644=CARTESIAN_POINT('Ctrl Pts',(0.152491794432586,0.122672995578315,
-0.398106413630828));
#24645=CARTESIAN_POINT('Ctrl Pts',(0.112388738317632,0.172532483800064,
-0.394442396761773));
#24646=CARTESIAN_POINT('Ctrl Pts',(0.0454752934615041,0.200814006580211,
-0.390778379892717));
#24647=CARTESIAN_POINT('Ctrl Pts',(-0.0182308640572237,0.194851488824733,
-0.387114363023661));
#24648=CARTESIAN_POINT('Ctrl Pts',(-0.0819370215759516,0.188888971069255,
-0.383450346154605));
#24649=CARTESIAN_POINT('Ctrl Pts',(-0.142435891757279,0.148682412778151,
-0.379786329285549));
#24650=CARTESIAN_POINT('Ctrl Pts',(-0.172596664765289,0.092255122594269,
-0.376122312416493));
#24651=CARTESIAN_POINT('Ctrl Pts',(-0.187602009772644,0.0641818713942949,
-0.374299420237359));
#24652=CARTESIAN_POINT('Ctrl Pts',(-0.195098125369958,0.0320936947925797,
-0.372476528058224));
#24653=CARTESIAN_POINT('Ctrl Pts',(-0.1950945860993,3.61475788830789E-6,
-0.37065363587909));
#24654=CARTESIAN_POINT('Origin',(0.,0.,-0.24));
#24655=CARTESIAN_POINT('',(-0.195607476207092,-0.000117485405063567,-0.290479697454244));
#24656=CARTESIAN_POINT('',(-0.195578322079833,-0.0001312749683362,-0.30065363587909));
#24657=CARTESIAN_POINT('',(-0.1954,-2.39295984553393E-17,-0.24));
#24658=CARTESIAN_POINT('Ctrl Pts',(-0.195607476207092,-0.000117485405063567,
-0.290479697454244));
#24659=CARTESIAN_POINT('Ctrl Pts',(-0.195201685186576,0.056545827244161,
-0.293720220029226));
#24660=CARTESIAN_POINT('Ctrl Pts',(-0.169152593581526,0.113534805853513,
-0.296960742604209));
#24661=CARTESIAN_POINT('Ctrl Pts',(-0.12580569557274,0.149911508696811,
-0.300201265179191));
#24662=CARTESIAN_POINT('Ctrl Pts',(-0.0767939198944633,0.191042175055213,
-0.303865282048247));
#24663=CARTESIAN_POINT('Ctrl Pts',(-0.0056677086826894,0.205821011997338,
-0.307529298917303));
#24664=CARTESIAN_POINT('Ctrl Pts',(0.0556722927194857,0.187619627746999,
-0.311193315786359));
#24665=CARTESIAN_POINT('Ctrl Pts',(0.11701229412166,0.169418243496659,-0.314857332655414));
#24666=CARTESIAN_POINT('Ctrl Pts',(0.168566085714236,0.118236638053856,
-0.31852134952447));
#24667=CARTESIAN_POINT('Ctrl Pts',(0.187211386887736,0.0570300966780328,
-0.322185366393526));
#24668=CARTESIAN_POINT('Ctrl Pts',(0.205856688061235,-0.00417644469779128,
-0.325849383262582));
#24669=CARTESIAN_POINT('Ctrl Pts',(0.191593498815658,-0.0754079220066363,
-0.329513400131638));
#24670=CARTESIAN_POINT('Ctrl Pts',(0.150818988166717,-0.124716363406268,
-0.333177417000694));
#24671=CARTESIAN_POINT('Ctrl Pts',(0.110044477517776,-0.174024804805899,
-0.33684143386975));
#24672=CARTESIAN_POINT('Ctrl Pts',(0.0427586454654721,-0.201410210296317,
-0.340505450738806));
#24673=CARTESIAN_POINT('Ctrl Pts',(-0.0208603338378075,-0.19459022297966,
-0.344169467607862));
#24674=CARTESIAN_POINT('Ctrl Pts',(-0.084479313141087,-0.187770235663004,
-0.347833484476918));
#24675=CARTESIAN_POINT('Ctrl Pts',(-0.144431439695342,-0.146744855539273,
-0.351497501345974));
#24676=CARTESIAN_POINT('Ctrl Pts',(-0.17382765481934,-0.0899138842095152,
-0.35516151821503));
#24677=CARTESIAN_POINT('Ctrl Pts',(-0.188050145833162,-0.0624178961840224,
-0.356934244628101));
#24678=CARTESIAN_POINT('Ctrl Pts',(-0.195120040035807,-0.0312220996446506,
-0.358706971041172));
#24679=CARTESIAN_POINT('Ctrl Pts',(-0.195096259697753,-1.61683889792347E-5,
-0.360479697454244));
#24680=CARTESIAN_POINT('Ctrl Pts',(-0.1950945860993,3.61475788830789E-6,
-0.37065363587909));
#24681=CARTESIAN_POINT('Ctrl Pts',(-0.195091011428967,-0.032407429257605,
-0.368812511189169));
#24682=CARTESIAN_POINT('Ctrl Pts',(-0.187437009001129,-0.0648204149726476,
-0.366971386499247));
#24683=CARTESIAN_POINT('Ctrl Pts',(-0.172142443533742,-0.0931006976602427,
-0.365130261809326));
#24684=CARTESIAN_POINT('Ctrl Pts',(-0.141704773459492,-0.149381205654212,
-0.36146624494027));
#24685=CARTESIAN_POINT('Ctrl Pts',(-0.0810067574762996,-0.18929419956549,
-0.357802228071214));
#24686=CARTESIAN_POINT('Ctrl Pts',(-0.0172728534882932,-0.194941042891399,
-0.354138211202158));
#24687=CARTESIAN_POINT('Ctrl Pts',(0.0464610504997132,-0.200587886217307,
-0.350474194333102));
#24688=CARTESIAN_POINT('Ctrl Pts',(0.113230842492533,-0.171968578957846,
-0.346810177464046));
#24689=CARTESIAN_POINT('Ctrl Pts',(0.153090248029826,-0.121917712582769,
-0.34314616059499));
#24690=CARTESIAN_POINT('Ctrl Pts',(0.192949653567118,-0.0718668462076918,
-0.339482143725934));
#24691=CARTESIAN_POINT('Ctrl Pts',(0.205898672648883,-0.000384420716998499,
-0.335818126856879));
#24692=CARTESIAN_POINT('Ctrl Pts',(0.186129314895087,0.0604684215793534,
-0.332154109987823));
#24693=CARTESIAN_POINT('Ctrl Pts',(0.16635995714129,0.121321263875706,-0.328490093118767));
#24694=CARTESIAN_POINT('Ctrl Pts',(0.11387222255193,0.171544522977716,-0.324826076249711));
#24695=CARTESIAN_POINT('Ctrl Pts',(0.0522073964039231,0.188613063308293,
-0.321162059380655));
#24696=CARTESIAN_POINT('Ctrl Pts',(-0.00945742974408397,0.205681603638869,
-0.317498042511599));
#24697=CARTESIAN_POINT('Ctrl Pts',(-0.0802993474507388,0.189595425198011,
-0.313834025642543));
#24698=CARTESIAN_POINT('Ctrl Pts',(-0.128545284234688,0.147569102657344,
-0.310170008773487));
#24699=CARTESIAN_POINT('Ctrl Pts',(-0.170314226307808,0.111184794490457,
-0.306997884475355));
#24700=CARTESIAN_POINT('Ctrl Pts',(-0.195146941473447,0.0553577293133787,
-0.303825760177223));
#24701=CARTESIAN_POINT('Ctrl Pts',(-0.195578322079833,-0.0001312749683362,
-0.30065363587909));
#24702=CARTESIAN_POINT('Origin',(0.,0.,-0.24));
#24703=CARTESIAN_POINT('',(-0.195363183094688,0.000168221922992429,-0.220479697454244));
#24704=CARTESIAN_POINT('',(-0.195397854366554,0.000168478207232705,-0.23065363587909));
#24705=CARTESIAN_POINT('',(-0.1954,-2.39295984553393E-17,-0.24));
#24706=CARTESIAN_POINT('Ctrl Pts',(-0.195363183094688,0.000168221922992429,
-0.220479697454244));
#24707=CARTESIAN_POINT('Ctrl Pts',(-0.195504269673892,0.0164080117818342,
-0.221405435279168));
#24708=CARTESIAN_POINT('Ctrl Pts',(-0.193644174979293,0.032615947390629,
-0.222331173104093));
#24709=CARTESIAN_POINT('Ctrl Pts',(-0.189655926211743,0.0482821032462058,
-0.223256910929018));
#24710=CARTESIAN_POINT('Ctrl Pts',(-0.173870667827724,0.110287843729762,
-0.226920927798073));
#24711=CARTESIAN_POINT('Ctrl Pts',(-0.124747222505265,0.163806438041988,
-0.230584944667129));
#24712=CARTESIAN_POINT('Ctrl Pts',(-0.0643178281358174,0.184834384063959,
-0.234248961536185));
#24713=CARTESIAN_POINT('Ctrl Pts',(-0.00388843376636972,0.205862330085929,
-0.237912978405241));
#24714=CARTESIAN_POINT('Ctrl Pts',(0.0678469096500664,0.194399627817645,
-0.241576995274297));
#24715=CARTESIAN_POINT('Ctrl Pts',(0.11871434919192,0.155587388833047,-0.245241012143353));
#24716=CARTESIAN_POINT('Ctrl Pts',(0.169581788733774,0.116775149848448,
-0.248905029012409));
#24717=CARTESIAN_POINT('Ctrl Pts',(0.199581324401046,0.0506133741475359,
-0.252569045881464));
#24718=CARTESIAN_POINT('Ctrl Pts',(0.195257935435045,-0.0132238767988385,
-0.25623306275052));
#24719=CARTESIAN_POINT('Ctrl Pts',(0.190934546469043,-0.0770611277452132,
-0.259897079619576));
#24720=CARTESIAN_POINT('Ctrl Pts',(0.152288232869768,-0.13857385393705,
-0.263561096488632));
#24721=CARTESIAN_POINT('Ctrl Pts',(0.0966521622178442,-0.170173123868098,
-0.267225113357688));
#24722=CARTESIAN_POINT('Ctrl Pts',(0.04101609156592,-0.201772393799146,
-0.270889130226744));
#24723=CARTESIAN_POINT('Ctrl Pts',(-0.0316097361386534,-0.203458207469406,
-0.2745531470958));
#24724=CARTESIAN_POINT('Ctrl Pts',(-0.088652081273832,-0.174474468983084,
-0.278217163964856));
#24725=CARTESIAN_POINT('Ctrl Pts',(-0.14569442640901,-0.145490730496762,
-0.281881180833912));
#24726=CARTESIAN_POINT('Ctrl Pts',(-0.187153288974794,-0.0858374398538568,
-0.285545197702967));
#24727=CARTESIAN_POINT('Ctrl Pts',(-0.194434050185296,-0.0222695466450644,
-0.289209214572023));
#24728=CARTESIAN_POINT('Ctrl Pts',(-0.195275574921494,-0.014922244211076,
-0.289632708866097));
#24729=CARTESIAN_POINT('Ctrl Pts',(-0.195660507833257,-0.00752264584909209,
-0.29005620316017));
#24730=CARTESIAN_POINT('Ctrl Pts',(-0.195607476207092,-0.000117485405063567,
-0.290479697454244));
#24731=CARTESIAN_POINT('Ctrl Pts',(-0.195578322079833,-0.0001312749683362,
-0.30065363587909));
#24732=CARTESIAN_POINT('Ctrl Pts',(-0.195645215081361,-0.00873580190638232,
-0.300161743308167));
#24733=CARTESIAN_POINT('Ctrl Pts',(-0.195125357252179,-0.0173321998828463,
-0.299669850737243));
#24734=CARTESIAN_POINT('Ctrl Pts',(-0.193990913268632,-0.0258467116936429,
-0.29917795816632));
#24735=CARTESIAN_POINT('Ctrl Pts',(-0.185540649657384,-0.0892697368634882,
-0.295513941297264));
#24736=CARTESIAN_POINT('Ctrl Pts',(-0.142990166573644,-0.148149320562704,
-0.291849924428208));
#24737=CARTESIAN_POINT('Ctrl Pts',(-0.0854237009492422,-0.1760775732527,
-0.288185907559152));
#24738=CARTESIAN_POINT('Ctrl Pts',(-0.0278572353248403,-0.204005825942696,
-0.284521890690096));
#24739=CARTESIAN_POINT('Ctrl Pts',(0.0447252128402237,-0.200982747623472,
-0.28085787382104));
#24740=CARTESIAN_POINT('Ctrl Pts',(0.0997698695794294,-0.168364183330645,
-0.277193856951985));
#24741=CARTESIAN_POINT('Ctrl Pts',(0.154814526318635,-0.135745619037819,
-0.273529840082929));
#24742=CARTESIAN_POINT('Ctrl Pts',(0.192321391631982,-0.0735315687713911,
-0.269865823213873));
#24743=CARTESIAN_POINT('Ctrl Pts',(0.195468343855467,-0.0096255258008377,
-0.266201806344817));
#24744=CARTESIAN_POINT('Ctrl Pts',(0.198615296078951,0.0542805171697163,
-0.262537789475761));
#24745=CARTESIAN_POINT('Ctrl Pts',(0.167402335212573,0.119878552844396,
-0.258873772606705));
#24746=CARTESIAN_POINT('Ctrl Pts',(0.11582871597203,0.157747367680544,-0.255209755737649));
#24747=CARTESIAN_POINT('Ctrl Pts',(0.0642550967314876,0.195616182516693,
-0.251545738868593));
#24748=CARTESIAN_POINT('Ctrl Pts',(-0.00767918088321898,0.20575577651431,
-0.247881721999537));
#24749=CARTESIAN_POINT('Ctrl Pts',(-0.0677110434843187,0.183618459739802,
-0.244217705130482));
#24750=CARTESIAN_POINT('Ctrl Pts',(-0.127742906085418,0.161481142965294,
-0.240553688261426));
#24751=CARTESIAN_POINT('Ctrl Pts',(-0.17587235367291,0.107066915418663,
-0.23688967139237));
#24752=CARTESIAN_POINT('Ctrl Pts',(-0.190512960004344,0.0447809775925131,
-0.233225654523314));
#24753=CARTESIAN_POINT('Ctrl Pts',(-0.193938700459235,0.0302067549031298,
-0.232368314975239));
#24754=CARTESIAN_POINT('Ctrl Pts',(-0.195530898725577,0.0152015494639044,
-0.231510975427165));
#24755=CARTESIAN_POINT('Ctrl Pts',(-0.195397854366554,0.000168478207232705,
-0.23065363587909));
#24756=CARTESIAN_POINT('Origin',(0.,0.,-0.24));
#24757=CARTESIAN_POINT('',(-0.195166600644982,-0.000111941290030684,-0.150479697454244));
#24758=CARTESIAN_POINT('',(-0.195146587185711,-9.71091332246861E-5,-0.16065363587909));
#24759=CARTESIAN_POINT('',(-0.1954,-2.39295984553393E-17,-0.24));
#24760=CARTESIAN_POINT('Ctrl Pts',(-0.195166600644982,-0.000111941290030684,
-0.150479697454244));
#24761=CARTESIAN_POINT('Ctrl Pts',(-0.194952618558542,0.0398988589954238,
-0.152754667398166));
#24762=CARTESIAN_POINT('Ctrl Pts',(-0.182960043012118,0.0800273756788333,
-0.155029637342089));
#24763=CARTESIAN_POINT('Ctrl Pts',(-0.160117027062204,0.112530200621256,
-0.157304607286012));
#24764=CARTESIAN_POINT('Ctrl Pts',(-0.123326564839096,0.164878540079165,
-0.160968624155068));
#24765=CARTESIAN_POINT('Ctrl Pts',(-0.0583904729961102,0.197446125267583,
-0.164632641024124));
#24766=CARTESIAN_POINT('Ctrl Pts',(0.0055670940850077,0.195626035987967,
-0.168296657893179));
#24767=CARTESIAN_POINT('Ctrl Pts',(0.0695246611661256,0.19380594670835,
-0.171960674762235));
#24768=CARTESIAN_POINT('Ctrl Pts',(0.132503703485376,0.157598182960699,
-0.175624691631291));
#24769=CARTESIAN_POINT('Ctrl Pts',(0.166257543654539,0.103242261140942,
-0.179288708500347));
#24770=CARTESIAN_POINT('Ctrl Pts',(0.200011383823701,0.0488863393211846,
-0.182952725369403));
#24771=CARTESIAN_POINT('Ctrl Pts',(0.204540021842776,-0.0236177405706785,
-0.186616742238459));
#24772=CARTESIAN_POINT('Ctrl Pts',(0.17781237832736,-0.0817513731146722,
-0.190280759107515));
#24773=CARTESIAN_POINT('Ctrl Pts',(0.151084734811943,-0.139885005658666,
-0.193944775976571));
#24774=CARTESIAN_POINT('Ctrl Pts',(0.0931008097620331,-0.183648190854791,
-0.197608792845626));
#24775=CARTESIAN_POINT('Ctrl Pts',(0.0298668118705716,-0.193412789202221,
-0.201272809714682));
#24776=CARTESIAN_POINT('Ctrl Pts',(-0.0333671860208894,-0.203177387549652,
-0.204936826583738));
#24777=CARTESIAN_POINT('Ctrl Pts',(-0.101851256753902,-0.178943399048388,
-0.208600843452794));
#24778=CARTESIAN_POINT('Ctrl Pts',(-0.14486975639762,-0.131579961470313,
-0.21226486032185));
#24779=CARTESIAN_POINT('Ctrl Pts',(-0.177019350761991,-0.0961832061569353,
-0.215003139365981));
#24780=CARTESIAN_POINT('Ctrl Pts',(-0.194945857138201,-0.0478681389712799,
-0.217741418410112));
#24781=CARTESIAN_POINT('Ctrl Pts',(-0.195363183094688,0.000168221922992429,
-0.220479697454244));
#24782=CARTESIAN_POINT('Ctrl Pts',(-0.195397854366554,0.000168478207232705,
-0.23065363587909));
#24783=CARTESIAN_POINT('Ctrl Pts',(-0.194962306296955,-0.049045372075947,
-0.227846958558109));
#24784=CARTESIAN_POINT('Ctrl Pts',(-0.176037076517356,-0.0985578644675523,
-0.225040281237128));
#24785=CARTESIAN_POINT('Ctrl Pts',(-0.142421832474098,-0.134225725993483,
-0.222233603916146));
#24786=CARTESIAN_POINT('Ctrl Pts',(-0.0985383335370456,-0.180788843647661,
-0.21856958704709));
#24787=CARTESIAN_POINT('Ctrl Pts',(-0.0296195705875667,-0.203757430850347,
-0.214905570178034));
#24788=CARTESIAN_POINT('Ctrl Pts',(0.0334238616745515,-0.19282989819453,
-0.211241553308979));
#24789=CARTESIAN_POINT('Ctrl Pts',(0.0964672939366692,-0.181902365538714,
-0.207577536439923));
#24790=CARTESIAN_POINT('Ctrl Pts',(0.153635395511427,-0.137078713024395,
-0.203913519570867));
#24791=CARTESIAN_POINT('Ctrl Pts',(0.179287838103686,-0.0784626953524838,
-0.200249502701811));
#24792=CARTESIAN_POINT('Ctrl Pts',(0.204940280695945,-0.0198466776805732,
-0.196585485832755));
#24793=CARTESIAN_POINT('Ctrl Pts',(0.199077064305706,0.0525617051489285,
-0.192921468963699));
#24794=CARTESIAN_POINT('Ctrl Pts',(0.164327880102392,0.106286744317414,
-0.189257452094643));
#24795=CARTESIAN_POINT('Ctrl Pts',(0.129578695899078,0.160011783485899,
-0.185593435225588));
#24796=CARTESIAN_POINT('Ctrl Pts',(0.0659435438826869,0.195053478993368,
-0.181929418356532));
#24797=CARTESIAN_POINT('Ctrl Pts',(0.00196328933688991,0.195695351501948,
-0.178265401487476));
#24798=CARTESIAN_POINT('Ctrl Pts',(-0.0620169652089071,0.196337224010529,
-0.17460138461842));
#24799=CARTESIAN_POINT('Ctrl Pts',(-0.12634232228411,0.162579273520222,
-0.170937367749364));
#24800=CARTESIAN_POINT('Ctrl Pts',(-0.162162389583139,0.109562219268833,
-0.167273350880308));
#24801=CARTESIAN_POINT('Ctrl Pts',(-0.183734218654723,0.0776338919811593,
-0.165066779213235));
#24802=CARTESIAN_POINT('Ctrl Pts',(-0.194967807817681,0.0387207125249729,
-0.162860207546163));
#24803=CARTESIAN_POINT('Ctrl Pts',(-0.195146587185711,-9.71091332246862E-5,
-0.16065363587909));
#24804=CARTESIAN_POINT('Origin',(0.,0.,-0.24));
#24805=CARTESIAN_POINT('',(-0.195709073584005,-9.38010969637637E-6,-0.0804796974542435));
#24806=CARTESIAN_POINT('',(-0.195698342875023,-3.28562868159645E-5,-0.0906536358790898));
#24807=CARTESIAN_POINT('',(-0.1954,-2.39295984553393E-17,-0.24));
#24808=CARTESIAN_POINT('Ctrl Pts',(-0.195709144608334,-9.38226522190222E-6,
-0.0804796974542435));
#24809=CARTESIAN_POINT('Ctrl Pts',(-0.195653902033672,0.0632821337469015,
-0.0841038995171643));
#24810=CARTESIAN_POINT('Ctrl Pts',(-0.162090188595658,0.126619703158733,
-0.0877281015800852));
#24811=CARTESIAN_POINT('Ctrl Pts',(-0.109671443000727,0.162085329147497,
-0.0913523036430061));
#24812=CARTESIAN_POINT('Ctrl Pts',(-0.0566768348690305,0.197940573871278,
-0.0950163205120619));
#24813=CARTESIAN_POINT('Ctrl Pts',(0.015589356712093,0.205308119443704,
-0.0986803373811178));
#24814=CARTESIAN_POINT('Ctrl Pts',(0.0747239197390152,0.18087830035279,
-0.102344354250174));
#24815=CARTESIAN_POINT('Ctrl Pts',(0.133858482765937,0.156448481261876,
-0.106008371119229));
#24816=CARTESIAN_POINT('Ctrl Pts',(0.179861417238658,0.100221297507622,
-0.109672387988285));
#24817=CARTESIAN_POINT('Ctrl Pts',(0.1920954828139,0.0374178292863625,-0.113336404857341));
#24818=CARTESIAN_POINT('Ctrl Pts',(0.204329548389143,-0.0253856389348972,
-0.117000421726397));
#24819=CARTESIAN_POINT('Ctrl Pts',(0.182794745066906,-0.0947653916231622,
-0.120664438595453));
#24820=CARTESIAN_POINT('Ctrl Pts',(0.137151991839732,-0.139605522577995,
-0.124328455464509));
#24821=CARTESIAN_POINT('Ctrl Pts',(0.0915092386125581,-0.184445653532828,
-0.127992472333565));
#24822=CARTESIAN_POINT('Ctrl Pts',(0.0217585354804476,-0.20474616275423,
-0.13165648920262));
#24823=CARTESIAN_POINT('Ctrl Pts',(-0.0408176472256261,-0.191401359750901,
-0.135320506071676));
#24824=CARTESIAN_POINT('Ctrl Pts',(-0.1033938299317,-0.178056556747573,
-0.138984522940732));
#24825=CARTESIAN_POINT('Ctrl Pts',(-0.158795492211738,-0.131066441519513,
-0.142648539809788));
#24826=CARTESIAN_POINT('Ctrl Pts',(-0.182173907050141,-0.0715068370417835,
-0.146312556678844));
#24827=CARTESIAN_POINT('Ctrl Pts',(-0.191036779795085,-0.0489274962749229,
-0.147701603603977));
#24828=CARTESIAN_POINT('Ctrl Pts',(-0.195297253430087,-0.0245416614527496,
-0.14909065052911));
#24829=CARTESIAN_POINT('Ctrl Pts',(-0.195166600644982,-0.000111941290030684,
-0.150479697454244));
#24830=CARTESIAN_POINT('Ctrl Pts',(-0.195146587185711,-9.71091332246862E-5,
-0.16065363587909));
#24831=CARTESIAN_POINT('Ctrl Pts',(-0.19526467133228,-0.0257363615406621,
-0.159196190677107));
#24832=CARTESIAN_POINT('Ctrl Pts',(-0.190559950845405,-0.0513340128677999,
-0.157738745475124));
#24833=CARTESIAN_POINT('Ctrl Pts',(-0.18082594422566,-0.0748498819709867,
-0.15628130027314));
#24834=CARTESIAN_POINT('Ctrl Pts',(-0.156354654046297,-0.133968770946947,
-0.152617283404085));
#24835=CARTESIAN_POINT('Ctrl Pts',(-0.100097296164716,-0.179930390886395,
-0.148953266535029));
#24836=CARTESIAN_POINT('Ctrl Pts',(-0.037285810874828,-0.192120531087848,
-0.145289249665973));
#24837=CARTESIAN_POINT('Ctrl Pts',(0.0255256744150603,-0.204310671289302,
-0.141625232796917));
#24838=CARTESIAN_POINT('Ctrl Pts',(0.0948912871132562,-0.182729331752761,
-0.137961215927861));
#24839=CARTESIAN_POINT('Ctrl Pts',(0.139700179401184,-0.137056046072734,
-0.134297199058805));
#24840=CARTESIAN_POINT('Ctrl Pts',(0.184509071689111,-0.0913827603927075,
-0.130633182189749));
#24841=CARTESIAN_POINT('Ctrl Pts',(0.20476124356677,-0.0216175285691954,
-0.126969165320693));
#24842=CARTESIAN_POINT('Ctrl Pts',(0.191373133778922,0.040949670807561,
-0.123305148451638));
#24843=CARTESIAN_POINT('Ctrl Pts',(0.177985023991073,0.103516870184318,
-0.119641131582582));
#24844=CARTESIAN_POINT('Ctrl Pts',(0.130956632537716,0.158886037114319,
-0.115977114713526));
#24845=CARTESIAN_POINT('Ctrl Pts',(0.0713811391615662,0.182223175406547,
-0.11231309784447));
#24846=CARTESIAN_POINT('Ctrl Pts',(0.011805645785417,0.205560313698776,
-0.108649080975414));
#24847=CARTESIAN_POINT('Ctrl Pts',(-0.0603169495135242,0.196865423353232,
-0.104985064106358));
#24848=CARTESIAN_POINT('Ctrl Pts',(-0.112640228305471,0.160039184697078,
-0.101321047237302));
#24849=CARTESIAN_POINT('Ctrl Pts',(-0.163418191256275,0.124300572261585,
-0.0977652434512315));
#24850=CARTESIAN_POINT('Ctrl Pts',(-0.195549073724041,0.062067736358378,
-0.0942094396651606));
#24851=CARTESIAN_POINT('Ctrl Pts',(-0.195698342875023,-3.28562868159645E-5,
-0.0906536358790898));
#24852=CARTESIAN_POINT('Origin',(0.,0.,-0.582472289227037));
#24853=CARTESIAN_POINT('',(-0.155796097460729,-7.46884010135441E-6,-0.0574722892270367));
#24854=CARTESIAN_POINT('',(-0.155389280676728,9.5162621374309E-5,-0.0436610441062962));
#24855=CARTESIAN_POINT('',(-0.15555,-2.84370958922189E-15,-0.582472289227037));
#24856=CARTESIAN_POINT('',(0.150444513166827,-0.0404002418790732,-0.0254000000000001));
#24857=CARTESIAN_POINT('Ctrl Pts',(-0.155796097460729,-7.46884010136202E-6,
-0.0574722892270367));
#24858=CARTESIAN_POINT('Ctrl Pts',(-0.155796580576894,-0.000560975889831939,
-0.0574324744209017));
#24859=CARTESIAN_POINT('Ctrl Pts',(-0.155542040915253,-0.0520513824587016,
-0.0537286427457109));
#24860=CARTESIAN_POINT('Ctrl Pts',(-0.0993493656725074,-0.153895266515289,
-0.0463607942014641));
#24861=CARTESIAN_POINT('Ctrl Pts',(0.068138238496685,-0.167299521168177,
-0.0357098459319202));
#24862=CARTESIAN_POINT('Ctrl Pts',(0.138167064954546,-0.0849802566602034,
-0.0287229145314322));
#24863=CARTESIAN_POINT('Ctrl Pts',(0.150444513166827,-0.0404002418790733,
-0.0254000000000001));
#24864=CARTESIAN_POINT('',(0.0106175386826097,-0.155187210724091,-0.0254000000000001));
#24865=CARTESIAN_POINT('Origin',(0.,0.,-0.0254000000000001));
#24866=CARTESIAN_POINT('Ctrl Pts',(-0.155389280676728,9.51626213743055E-5,
-0.0436610441062962));
#24867=CARTESIAN_POINT('Ctrl Pts',(-0.15512974883406,-0.0338312999427815,
-0.0412380462732533));
#24868=CARTESIAN_POINT('Ctrl Pts',(-0.127591546791687,-0.119392150871042,
-0.0351510315711546));
#24869=CARTESIAN_POINT('Ctrl Pts',(-0.0404206461299352,-0.158679121552366,
-0.029064016869056));
#24870=CARTESIAN_POINT('Ctrl Pts',(0.0106175386826097,-0.155187210724091,
-0.0254000000000001));
#24871=CARTESIAN_POINT('Origin',(0.,0.,-0.582472289227037));
#24872=CARTESIAN_POINT('',(-0.155364200257559,-8.91119123082438E-5,-0.127472289227037));
#24873=CARTESIAN_POINT('',(-0.155787498639764,-2.6155554834012E-5,-0.113661044106296));
#24874=CARTESIAN_POINT('',(-0.15555,-2.84370958922189E-15,-0.582472289227037));
#24875=CARTESIAN_POINT('Ctrl Pts',(-0.155364200257559,-8.91119123082353E-5,
-0.127472289227037));
#24876=CARTESIAN_POINT('Ctrl Pts',(-0.155468207630757,-0.0195366194420458,
-0.126083242301904));
#24877=CARTESIAN_POINT('Ctrl Pts',(-0.143130308880635,-0.0901555192989463,
-0.121030178507715));
#24878=CARTESIAN_POINT('Ctrl Pts',(-0.038204614525159,-0.179150510879271,
-0.11231309784447));
#24879=CARTESIAN_POINT('Ctrl Pts',(0.128372486890396,-0.130669279414751,
-0.101321047237302));
#24880=CARTESIAN_POINT('Ctrl Pts',(0.179801432490814,0.0350219262760309,
-0.0903289966301345));
#24881=CARTESIAN_POINT('Ctrl Pts',(0.0699382320215437,0.169302454929678,
-0.0793369460229671));
#24882=CARTESIAN_POINT('Ctrl Pts',(-0.10202117751736,0.151771175659713,
-0.0683847102219343));
#24883=CARTESIAN_POINT('Ctrl Pts',(-0.1557521210918,0.050376335231986,-0.0610964912899576));
#24884=CARTESIAN_POINT('Ctrl Pts',(-0.155796097460729,-7.46884010136202E-6,
-0.0574722892270367));
#24885=CARTESIAN_POINT('Ctrl Pts',(-0.155787498639764,-2.61555548340198E-5,
-0.113661044106296));
#24886=CARTESIAN_POINT('Ctrl Pts',(-0.155791114881889,-0.00153062434586674,
-0.113552831023311));
#24887=CARTESIAN_POINT('Ctrl Pts',(-0.155095219214847,-0.0539719215336349,
-0.10978060107127));
#24888=CARTESIAN_POINT('Ctrl Pts',(-0.0965231054289514,-0.155685461973447,
-0.102344354250173));
#24889=CARTESIAN_POINT('Ctrl Pts',(0.0766264864264418,-0.166372403162464,
-0.091352303643006));
#24890=CARTESIAN_POINT('Ctrl Pts',(0.181065301238179,-0.0278415620581252,
-0.0803602530358381));
#24891=CARTESIAN_POINT('Ctrl Pts',(0.123039270360697,0.135703326763709,
-0.0693682024286707));
#24892=CARTESIAN_POINT('Ctrl Pts',(-0.0452659821533855,0.177444214884968,
-0.058376151821503));
#24893=CARTESIAN_POINT('Ctrl Pts',(-0.144950921528674,0.0860145677096474,
-0.0498070990473782));
#24894=CARTESIAN_POINT('Ctrl Pts',(-0.155522208553431,0.017471730314721,
-0.0449020631423093));
#24895=CARTESIAN_POINT('Ctrl Pts',(-0.155389280676728,9.51626213743055E-5,
-0.0436610441062962));
#24896=CARTESIAN_POINT('Origin',(0.,0.,-0.582472289227037));
#24897=CARTESIAN_POINT('',(-0.155520691557721,0.000133914637262764,-0.197472289227037));
#24898=CARTESIAN_POINT('',(-0.155348268355872,-7.73046349714923E-5,-0.183661044106296));
#24899=CARTESIAN_POINT('',(-0.15555,-2.84370958922189E-15,-0.582472289227037));
#24900=CARTESIAN_POINT('Ctrl Pts',(-0.155520691557721,0.000133914637262762,
-0.197472289227037));
#24901=CARTESIAN_POINT('Ctrl Pts',(-0.155188475321633,-0.0381058803325632,
-0.194734010182906));
#24902=CARTESIAN_POINT('Ctrl Pts',(-0.121822858612577,-0.128032047716084,
-0.188331714269719));
#24903=CARTESIAN_POINT('Ctrl Pts',(0.0279551249589101,-0.181032955704809,
-0.178265401487475));
#24904=CARTESIAN_POINT('Ctrl Pts',(0.166431064695553,-0.0765186753989169,
-0.167273350880308));
#24905=CARTESIAN_POINT('Ctrl Pts',(0.15561587057272,0.0966339800849018,
-0.15628130027314));
#24906=CARTESIAN_POINT('Ctrl Pts',(0.00521070118542118,0.183104568379892,
-0.145289249665973));
#24907=CARTESIAN_POINT('Ctrl Pts',(-0.130271184964665,0.115155947767654,
-0.135686245983938));
#24908=CARTESIAN_POINT('Ctrl Pts',(-0.15519385781362,0.03176186037225,-0.12974725917096));
#24909=CARTESIAN_POINT('Ctrl Pts',(-0.155364200257559,-8.91119123082353E-5,
-0.127472289227037));
#24910=CARTESIAN_POINT('Ctrl Pts',(-0.155348268355872,-7.73046349714958E-5,
-0.183661044106296));
#24911=CARTESIAN_POINT('Ctrl Pts',(-0.155442270346654,-0.0204876716358764,
-0.182203598904313));
#24912=CARTESIAN_POINT('Ctrl Pts',(-0.142281509160764,-0.0920933232311109,
-0.177082136833274));
#24913=CARTESIAN_POINT('Ctrl Pts',(-0.0348991934490358,-0.179823450787922,
-0.168296657893179));
#24914=CARTESIAN_POINT('Ctrl Pts',(0.130758243427182,-0.128283368419821,
-0.157304607286012));
#24915=CARTESIAN_POINT('Ctrl Pts',(0.179124036706147,0.0383284300983071,
-0.146312556678844));
#24916=CARTESIAN_POINT('Ctrl Pts',(0.0668118623371123,0.17055986176609,
-0.135320506071676));
#24917=CARTESIAN_POINT('Ctrl Pts',(-0.103734078699234,0.149999339088803,
-0.124436668547494));
#24918=CARTESIAN_POINT('Ctrl Pts',(-0.155668671534159,0.0494096028175303,
-0.117216847892367));
#24919=CARTESIAN_POINT('Ctrl Pts',(-0.155787498639764,-2.61555548340198E-5,
-0.113661044106296));
#24920=CARTESIAN_POINT('Origin',(0.,0.,-0.582472289227037));
#24921=CARTESIAN_POINT('',(-0.155715163377754,-9.35253570008701E-5,-0.267472289227037));
#24922=CARTESIAN_POINT('',(-0.155548291948401,0.000134118654731868,-0.253661044106296));
#24923=CARTESIAN_POINT('',(-0.15555,-2.84370958922189E-15,-0.582472289227037));
#24924=CARTESIAN_POINT('Ctrl Pts',(-0.155715163377754,-9.35253570008522E-5,
-0.267472289227037));
#24925=CARTESIAN_POINT('Ctrl Pts',(-0.155757379700425,-0.00598847268079084,
-0.267048794932964));
#24926=CARTESIAN_POINT('Ctrl Pts',(-0.152799763003076,-0.0628429920017419,
-0.262961283769834));
#24927=CARTESIAN_POINT('Ctrl Pts',(-0.0829776968055973,-0.163306819284929,
-0.255209755737649));
#24928=CARTESIAN_POINT('Ctrl Pts',(0.0904657141377962,-0.159280796003317,
-0.244217705130481));
#24929=CARTESIAN_POINT('Ctrl Pts',(0.182759993774958,-0.0123774506736319,
-0.233225654523314));
#24930=CARTESIAN_POINT('Ctrl Pts',(0.111115759797821,0.145628652861839,
-0.222233603916146));
#24931=CARTESIAN_POINT('Ctrl Pts',(-0.0602010160736213,0.173003627342364,
-0.211241553308979));
#24932=CARTESIAN_POINT('Ctrl Pts',(-0.148291552645345,0.0770314971592852,
-0.202987781745942));
#24933=CARTESIAN_POINT('Ctrl Pts',(-0.15563300485043,0.0130617514465919,
-0.198398027051962));
#24934=CARTESIAN_POINT('Ctrl Pts',(-0.155520691557721,0.000133914637262762,
-0.197472289227037));
#24935=CARTESIAN_POINT('Ctrl Pts',(-0.155548291948401,0.00013411865473186,
-0.253661044106296));
#24936=CARTESIAN_POINT('Ctrl Pts',(-0.155201569828512,-0.0390430277707979,
-0.250854366785315));
#24937=CARTESIAN_POINT('Ctrl Pts',(-0.120468353035836,-0.129912631585972,
-0.244383672595278));
#24938=CARTESIAN_POINT('Ctrl Pts',(0.031284490132526,-0.180487370051941,
-0.234248961536185));
#24939=CARTESIAN_POINT('Ctrl Pts',(0.167812098115434,-0.0734405049249859,
-0.223256910929018));
#24940=CARTESIAN_POINT('Ctrl Pts',(0.15380969315891,0.0994836089306307,
-0.21226486032185));
#24941=CARTESIAN_POINT('Ctrl Pts',(0.00183761696418741,0.183169418595726,
-0.201272809714682));
#24942=CARTESIAN_POINT('Ctrl Pts',(-0.131414133088497,0.113238893752059,
-0.191738204309498));
#24943=CARTESIAN_POINT('Ctrl Pts',(-0.155205949365611,0.0308239858406309,
-0.185867615773369));
#24944=CARTESIAN_POINT('Ctrl Pts',(-0.155348268355872,-7.73046349714958E-5,
-0.183661044106296));
#24945=CARTESIAN_POINT('Origin',(0.,0.,-0.582472289227037));
#24946=CARTESIAN_POINT('',(-0.155308204687746,-1.28709974709959E-5,-0.337472289227037));
#24947=CARTESIAN_POINT('',(-0.15569195496171,-0.000104502667989975,-0.323661044106296));
#24948=CARTESIAN_POINT('',(-0.15555,-2.84370958922189E-15,-0.582472289227037));
#24949=CARTESIAN_POINT('Ctrl Pts',(-0.155308204687746,-1.28709974709911E-5,
-0.337472289227037));
#24950=CARTESIAN_POINT('Ctrl Pts',(-0.155327135248565,-0.0248546448297111,
-0.335699562813965));
#24951=CARTESIAN_POINT('Ctrl Pts',(-0.138066551401952,-0.101016698517625,
-0.330262819531838));
#24952=CARTESIAN_POINT('Ctrl Pts',(-0.0195250965894654,-0.182134892710474,
-0.321162059380655));
#24953=CARTESIAN_POINT('Ctrl Pts',(0.141165453703306,-0.116733667162349,
-0.310170008773487));
#24954=CARTESIAN_POINT('Ctrl Pts',(0.175228489841733,0.0533797867075198,
-0.29917795816632));
#24955=CARTESIAN_POINT('Ctrl Pts',(0.052108853983618,0.175610575755033,
-0.288185907559152));
#24956=CARTESIAN_POINT('Ctrl Pts',(-0.111208875107151,0.141675883510508,
-0.277617351246058));
#24957=CARTESIAN_POINT('Ctrl Pts',(-0.155392129635476,0.0450138353522466,
-0.270712811802019));
#24958=CARTESIAN_POINT('Ctrl Pts',(-0.155715163377754,-9.35253570008522E-5,
-0.267472289227037));
#24959=CARTESIAN_POINT('Ctrl Pts',(-0.15569195496171,-0.000104502667989961,
-0.323661044106296));
#24960=CARTESIAN_POINT('Ctrl Pts',(-0.155745205762056,-0.00695421692189423,
-0.323169151535373));
#24961=CARTESIAN_POINT('Ctrl Pts',(-0.152248767557636,-0.0647715135328056,
-0.319013242095394));
#24962=CARTESIAN_POINT('Ctrl Pts',(-0.0799559507003814,-0.164807298147092,
-0.311193315786359));
#24963=CARTESIAN_POINT('Ctrl Pts',(0.0933838621769322,-0.157587648721984,
-0.300201265179191));
#24964=CARTESIAN_POINT('Ctrl Pts',(0.182956936375875,-0.00900941659901149,
-0.289209214572024));
#24965=CARTESIAN_POINT('Ctrl Pts',(0.108414826916839,0.14765037535385,-0.278217163964856));
#24966=CARTESIAN_POINT('Ctrl Pts',(-0.0633770392495001,0.17186553164345,
-0.267225113357688));
#24967=CARTESIAN_POINT('Ctrl Pts',(-0.148969863825595,0.0750959307795305,
-0.259039740071501));
#24968=CARTESIAN_POINT('Ctrl Pts',(-0.155654203156415,0.0121013358193961,
-0.254518383654371));
#24969=CARTESIAN_POINT('Ctrl Pts',(-0.155548291948401,0.00013411865473186,
-0.253661044106296));
#24970=CARTESIAN_POINT('Origin',(0.,0.,-0.582472289227037));
#24971=CARTESIAN_POINT('',(-0.155671978531511,0.000121856215612283,-0.407472289227037));
#24972=CARTESIAN_POINT('',(-0.155306872404023,2.8775618683835E-6,-0.393661044106296));
#24973=CARTESIAN_POINT('',(-0.15555,-2.84370958922189E-15,-0.582472289227037));
#24974=CARTESIAN_POINT('Ctrl Pts',(-0.155671978531511,0.000121856215612291,
-0.407472289227037));
#24975=CARTESIAN_POINT('Ctrl Pts',(-0.15531801647687,-0.0433643059521865,
-0.404350330694967));
#24976=CARTESIAN_POINT('Ctrl Pts',(-0.113858398180907,-0.138508424000405,
-0.397564355293842));
#24977=CARTESIAN_POINT('Ctrl Pts',(0.0464781498992043,-0.177175601660564,
-0.38711436302366));
#24978=CARTESIAN_POINT('Ctrl Pts',(0.17343439203133,-0.0589507354003139,
-0.376122312416494));
#24979=CARTESIAN_POINT('Ctrl Pts',(0.144820268191827,0.112170318563691,
-0.365130261809325));
#24980=CARTESIAN_POINT('Ctrl Pts',(-0.0137013956641988,0.182664248636804,
-0.354138211202158));
#24981=CARTESIAN_POINT('Ctrl Pts',(-0.136348787789886,0.104365623877948,
-0.344918887008062));
#24982=CARTESIAN_POINT('Ctrl Pts',(-0.155288008007231,0.0264903781289625,
-0.339363579683021));
#24983=CARTESIAN_POINT('Ctrl Pts',(-0.155308204687746,-1.28709974709911E-5,
-0.337472289227037));
#24984=CARTESIAN_POINT('Ctrl Pts',(-0.155306872404023,2.87756186839044E-6,
-0.393661044106296));
#24985=CARTESIAN_POINT('Ctrl Pts',(-0.155304026754226,-0.0257982375691955,
-0.391819919416375));
#24986=CARTESIAN_POINT('Ctrl Pts',(-0.137085244699405,-0.102950698396822,
-0.386314777857398));
#24987=CARTESIAN_POINT('Ctrl Pts',(-0.016166963865162,-0.182462532985216,
-0.377145619429364));
#24988=CARTESIAN_POINT('Ctrl Pts',(0.143291190860782,-0.114114530259385,
-0.366153568822197));
#24989=CARTESIAN_POINT('Ctrl Pts',(0.174215754599295,0.0565982325616605,
-0.35516151821503));
#24990=CARTESIAN_POINT('Ctrl Pts',(0.0488656965331514,0.176540319869506,
-0.344169467607861));
#24991=CARTESIAN_POINT('Ctrl Pts',(-0.112746501248559,0.139842800436154,
-0.333669309571618));
#24992=CARTESIAN_POINT('Ctrl Pts',(-0.155348550389943,0.0440680388674291,
-0.326833168404429));
#24993=CARTESIAN_POINT('Ctrl Pts',(-0.15569195496171,-0.000104502667989961,
-0.323661044106296));
#24994=CARTESIAN_POINT('Origin',(2.59090492670967E-17,0.,-0.0254000000000001));
#24995=CARTESIAN_POINT('',(-0.044842238767986,0.190184998415424,-0.0254000000000001));
#24996=CARTESIAN_POINT('Ctrl Pts',(0.150444513166827,-0.0404002418790722,
-0.0254));
#24997=CARTESIAN_POINT('Ctrl Pts',(0.152288523601877,-0.0359477914915009,
-0.0254));
#24998=CARTESIAN_POINT('Ctrl Pts',(0.153909584332356,-0.0314161192062029,
-0.0254));
#24999=CARTESIAN_POINT('Ctrl Pts',(0.155297293824378,-0.0268185318320736,
-0.0254));
#25000=CARTESIAN_POINT('Ctrl Pts',(0.157109245974868,-0.0208153961775976,
-0.0254));
#25001=CARTESIAN_POINT('Ctrl Pts',(0.158523650087112,-0.0146999624105404,
-0.0254));
#25002=CARTESIAN_POINT('Ctrl Pts',(0.159556946383489,-0.00850639978364366,
-0.0254));
#25003=CARTESIAN_POINT('Ctrl Pts',(0.160489936122728,-0.00291407316784563,
-0.0254));
#25004=CARTESIAN_POINT('Ctrl Pts',(0.161111867808762,0.00274714571770028,
-0.0254000000000003));
#25005=CARTESIAN_POINT('Ctrl Pts',(0.161430884359787,0.00842270596691387,
-0.0254000000000002));
#25006=CARTESIAN_POINT('Ctrl Pts',(0.161919051332622,0.0171075878550349,
-0.0254000000000001));
#25007=CARTESIAN_POINT('Ctrl Pts',(0.161701943773179,0.0258371679676822,
-0.0254000000000001));
#25008=CARTESIAN_POINT('Ctrl Pts',(0.160816263117086,0.0345264326241675,
-0.0254000000000001));
#25009=CARTESIAN_POINT('Ctrl Pts',(0.160262807613304,0.0399562919248784,
-0.0254000000000001));
#25010=CARTESIAN_POINT('Ctrl Pts',(0.159446308044253,0.0453760768932331,
-0.0254000000000002));
#25011=CARTESIAN_POINT('Ctrl Pts',(0.158380032328247,0.0507336350772083,
-0.0254000000000001));
#25012=CARTESIAN_POINT('Ctrl Pts',(0.156098217349856,0.0621987339519919,
-0.0254000000000001));
#25013=CARTESIAN_POINT('Ctrl Pts',(0.152675969965111,0.0734017680619525,
-0.0254));
#25014=CARTESIAN_POINT('Ctrl Pts',(0.148188225310357,0.084152422306617,
-0.0254));
#25015=CARTESIAN_POINT('Ctrl Pts',(0.146120109284199,0.0891067149514794,
-0.0254));
#25016=CARTESIAN_POINT('Ctrl Pts',(0.143824981035637,0.093965065234332,
-0.0254000000000001));
#25017=CARTESIAN_POINT('Ctrl Pts',(0.14130650146901,0.0987086415880662,
-0.0254000000000001));
#25018=CARTESIAN_POINT('Ctrl Pts',(0.13912884558959,0.102810273808185,-0.0254000000000001));
#25019=CARTESIAN_POINT('Ctrl Pts',(0.136781562604662,0.106829358853639,
-0.0253999999999999));
#25020=CARTESIAN_POINT('Ctrl Pts',(0.134281947115991,0.110730142526631,
-0.0253999999999999));
#25021=CARTESIAN_POINT('Ctrl Pts',(0.130254692328574,0.117014889037818,
-0.0253999999999999));
#25022=CARTESIAN_POINT('Ctrl Pts',(0.125827047154186,0.123004551843775,
-0.0254));
#25023=CARTESIAN_POINT('Ctrl Pts',(0.121015339265292,0.128651930926206,
-0.0254));
#25024=CARTESIAN_POINT('Ctrl Pts',(0.115989939416535,0.134550114823078,
-0.0254));
#25025=CARTESIAN_POINT('Ctrl Pts',(0.110545683683119,0.140075249109618,
-0.0254000000000001));
#25026=CARTESIAN_POINT('Ctrl Pts',(0.104735241535896,0.145219293087094,
-0.0254000000000001));
#25027=CARTESIAN_POINT('Ctrl Pts',(0.101154909616182,0.148388997626321,
-0.0254000000000001));
#25028=CARTESIAN_POINT('Ctrl Pts',(0.09743534991764,0.151413906784189,-0.0254));
#25029=CARTESIAN_POINT('Ctrl Pts',(0.0935873754776157,0.154290981378466,
-0.0254));
#25030=CARTESIAN_POINT('Ctrl Pts',(0.0905644815369063,0.156551155268278,
-0.0253999999999999));
#25031=CARTESIAN_POINT('Ctrl Pts',(0.0874690119107099,0.158714939473109,
-0.0253999999999999));
#25032=CARTESIAN_POINT('Ctrl Pts',(0.0843113769815779,0.16077906433524,
-0.0253999999999999));
#25033=CARTESIAN_POINT('Ctrl Pts',(0.0749099637749328,0.166924705352815,
-0.0253999999999999));
#25034=CARTESIAN_POINT('Ctrl Pts',(0.0649487520954266,0.172196873794768,
-0.0254000000000001));
#25035=CARTESIAN_POINT('Ctrl Pts',(0.0545782856068879,0.17657123368835,
-0.0254000000000002));
#25036=CARTESIAN_POINT('Ctrl Pts',(0.0469628838054677,0.179783481493254,
-0.0254000000000003));
#25037=CARTESIAN_POINT('Ctrl Pts',(0.0391259623884753,0.182511210134655,
-0.0254));
#25038=CARTESIAN_POINT('Ctrl Pts',(0.0311192198383689,0.18473535989345,
-0.0254));
#25039=CARTESIAN_POINT('Ctrl Pts',(0.0279473244497433,0.185616463578174,
-0.0254));
#25040=CARTESIAN_POINT('Ctrl Pts',(0.0247505316468867,0.186417770388197,
-0.0254));
#25041=CARTESIAN_POINT('Ctrl Pts',(0.0215412556878254,0.187136369631423,
-0.0254));
#25042=CARTESIAN_POINT('Ctrl Pts',(0.00902611956062844,0.189938673784945,
-0.0254));
#25043=CARTESIAN_POINT('Ctrl Pts',(-0.00371436117299067,0.191497453815457,
-0.0254000000000002));
#25044=CARTESIAN_POINT('Ctrl Pts',(-0.0164851355348781,0.191763125459253,
-0.0254000000000003));
#25045=CARTESIAN_POINT('Ctrl Pts',(-0.0259446175737208,0.191959911971292,
-0.0254000000000003));
#25046=CARTESIAN_POINT('Ctrl Pts',(-0.0354216684714881,0.19144650970575,
-0.0254000000000001));
#25047=CARTESIAN_POINT('Ctrl Pts',(-0.044842238767986,0.190184998415424,
-0.0254000000000001));
#25048=CARTESIAN_POINT('',(-0.1954,-2.39295984553393E-17,-0.0254000000000001));
#25049=CARTESIAN_POINT('Origin',(0.,0.,-0.0254000000000001));
#25050=CARTESIAN_POINT('',(-0.178079963314484,0.080770315425888,-0.0254000000000001));
#25051=CARTESIAN_POINT('Origin',(0.,0.,-0.0254000000000001));
#25052=CARTESIAN_POINT('Ctrl Pts',(-0.178226250896966,0.0807893643570701,
-0.0254000000000002));
#25053=CARTESIAN_POINT('Ctrl Pts',(-0.180177392099784,0.0751485900811471,
-0.0254000000000002));
#25054=CARTESIAN_POINT('Ctrl Pts',(-0.181850551972504,0.0694252034091049,
-0.0254000000000002));
#25055=CARTESIAN_POINT('Ctrl Pts',(-0.183229787629028,0.0636315522952145,
-0.0254000000000002));
#25056=CARTESIAN_POINT('Ctrl Pts',(-0.18542372495759,0.0544156453634958,
-0.0254000000000003));
#25057=CARTESIAN_POINT('Ctrl Pts',(-0.186874660056435,0.045021678959618,
-0.0254000000000002));
#25058=CARTESIAN_POINT('Ctrl Pts',(-0.187601227544073,0.0355338426658405,
-0.0254000000000001));
#25059=CARTESIAN_POINT('Ctrl Pts',(-0.187947943303617,0.0310062765099001,
-0.0254000000000001));
#25060=CARTESIAN_POINT('Ctrl Pts',(-0.188129147364736,0.026457242532671,
-0.0254000000000002));
#25061=CARTESIAN_POINT('Ctrl Pts',(-0.188146660120574,0.0219107093455789,
-0.0254000000000002));
#25062=CARTESIAN_POINT('Ctrl Pts',(-0.188174227502584,0.0147538678781792,
-0.0254000000000002));
#25063=CARTESIAN_POINT('Ctrl Pts',(-0.187797349460741,0.00759407962602553,
-0.0254000000000002));
#25064=CARTESIAN_POINT('Ctrl Pts',(-0.187024335822518,0.000468048982504179,
-0.0254000000000002));
#25065=CARTESIAN_POINT('Ctrl Pts',(-0.186499030634634,-0.00437447989534716,
-0.0254000000000002));
#25066=CARTESIAN_POINT('Ctrl Pts',(-0.185790682000941,-0.00920140104915156,
-0.0254000000000003));
#25067=CARTESIAN_POINT('Ctrl Pts',(-0.184900643419175,-0.0140005797065861,
-0.0254000000000003));
#25068=CARTESIAN_POINT('Ctrl Pts',(-0.184132779193588,-0.0181409817955999,
-0.0254000000000003));
#25069=CARTESIAN_POINT('Ctrl Pts',(-0.183229102993718,-0.0222617381008127,
-0.0254000000000004));
#25070=CARTESIAN_POINT('Ctrl Pts',(-0.182194971678485,-0.0263383737172839,
-0.0254000000000003));
#25071=CARTESIAN_POINT('Ctrl Pts',(-0.179181975057578,-0.0382158685345879,
-0.0254000000000003));
#25072=CARTESIAN_POINT('Ctrl Pts',(-0.175059469051961,-0.0497546103305461,
-0.0254000000000002));
#25073=CARTESIAN_POINT('Ctrl Pts',(-0.169859086925564,-0.0607628510176612,
-0.0254000000000002));
#25074=CARTESIAN_POINT('Ctrl Pts',(-0.167269936719285,-0.0662435999228502,
-0.0254000000000001));
#25075=CARTESIAN_POINT('Ctrl Pts',(-0.164412932388428,-0.0715924281006022,
-0.0254000000000001));
#25076=CARTESIAN_POINT('Ctrl Pts',(-0.161288438287051,-0.0767821423128327,
-0.0254000000000002));
#25077=CARTESIAN_POINT('Ctrl Pts',(-0.158668603425435,-0.0811336289131844,
-0.0254000000000002));
#25078=CARTESIAN_POINT('Ctrl Pts',(-0.155857058035564,-0.0853773956860439,
-0.0254000000000001));
#25079=CARTESIAN_POINT('Ctrl Pts',(-0.152872677055221,-0.0894708909542363,
-0.0254000000000001));
#25080=CARTESIAN_POINT('Ctrl Pts',(-0.148577680288583,-0.0953620787941746,
-0.0254000000000002));
#25081=CARTESIAN_POINT('Ctrl Pts',(-0.143920174645333,-0.100952225610252,
-0.0254000000000002));
#25082=CARTESIAN_POINT('Ctrl Pts',(-0.138904565814662,-0.106196500366509,
-0.0254000000000002));
#25083=CARTESIAN_POINT('Ctrl Pts',(-0.133141847811386,-0.112221945645895,
-0.0254000000000001));
#25084=CARTESIAN_POINT('Ctrl Pts',(-0.126906212836165,-0.117791094215227,
-0.0254000000000001));
#25085=CARTESIAN_POINT('Ctrl Pts',(-0.120262137870373,-0.122877728119754,
-0.0254000000000001));
#25086=CARTESIAN_POINT('Ctrl Pts',(-0.117196150482267,-0.125225015812847,
-0.0254000000000001));
#25087=CARTESIAN_POINT('Ctrl Pts',(-0.114043125364532,-0.127469381869944,
-0.0254));
#25088=CARTESIAN_POINT('Ctrl Pts',(-0.110809234819109,-0.129607334440998,
-0.0254));
#25089=CARTESIAN_POINT('Ctrl Pts',(-0.107698297930514,-0.131664001302767,
-0.0254));
#25090=CARTESIAN_POINT('Ctrl Pts',(-0.104518672572365,-0.133617962067455,
-0.0254000000000002));
#25091=CARTESIAN_POINT('Ctrl Pts',(-0.101282336137666,-0.135464061965196,
-0.0254000000000002));
#25092=CARTESIAN_POINT('Ctrl Pts',(-0.0928811385341354,-0.140256348042283,
-0.0254000000000002));
#25093=CARTESIAN_POINT('Ctrl Pts',(-0.084085973651599,-0.144331678880361,
-0.0254000000000001));
#25094=CARTESIAN_POINT('Ctrl Pts',(-0.075000622341404,-0.147649433262726,
-0.0254000000000001));
#25095=CARTESIAN_POINT('Ctrl Pts',(-0.0691135240229781,-0.149799261659946,
-0.0254000000000002));
#25096=CARTESIAN_POINT('Ctrl Pts',(-0.0631044080958086,-0.151630500595275,
-0.0254));
#25097=CARTESIAN_POINT('Ctrl Pts',(-0.0570016890090982,-0.153126178223591,
-0.0254));
#25098=CARTESIAN_POINT('Ctrl Pts',(-0.0525695195872538,-0.15421243117985,
-0.0254));
#25099=CARTESIAN_POINT('Ctrl Pts',(-0.0480836796866101,-0.155121871124085,
-0.0254000000000002));
#25100=CARTESIAN_POINT('Ctrl Pts',(-0.0435831167051402,-0.155843198108109,
-0.0254000000000002));
#25101=CARTESIAN_POINT('Ctrl Pts',(-0.032940985490312,-0.157548863920228,
-0.0254000000000002));
#25102=CARTESIAN_POINT('Ctrl Pts',(-0.0221883550620207,-0.158214788306086,
-0.0254000000000002));
#25103=CARTESIAN_POINT('Ctrl Pts',(-0.0114741912448819,-0.15776348171624,
-0.0254000000000002));
#25104=CARTESIAN_POINT('Ctrl Pts',(-0.00407369102796414,-0.157451754681536,
-0.0254000000000002));
#25105=CARTESIAN_POINT('Ctrl Pts',(0.00330847097457228,-0.156606036832058,
-0.0254000000000001));
#25106=CARTESIAN_POINT('Ctrl Pts',(0.0106175386826097,-0.155187210724091,
-0.0254000000000001));
#25107=CARTESIAN_POINT('Ctrl Pts',(-0.0685825729128711,0.139614588036676,
-0.476074074893873));
#25108=CARTESIAN_POINT('Ctrl Pts',(-0.11449921200636,0.117059056463457,
-0.472410058024817));
#25109=CARTESIAN_POINT('Ctrl Pts',(-0.181611195120813,0.0235386823327614,
-0.465082024286706));
#25110=CARTESIAN_POINT('Ctrl Pts',(-0.119678168822871,-0.138828443538179,
-0.454089973679538));
#25111=CARTESIAN_POINT('Ctrl Pts',(0.0497528850778061,-0.176238783935,-0.443097923072371));
#25112=CARTESIAN_POINT('Ctrl Pts',(0.174480439215212,-0.0557730335995584,
-0.432105872465203));
#25113=CARTESIAN_POINT('Ctrl Pts',(0.142735182152908,0.114832328488475,
-0.421113821858035));
#25114=CARTESIAN_POINT('Ctrl Pts',(-0.017066041194646,0.182373641719569,
-0.410121771250868));
#25115=CARTESIAN_POINT('Ctrl Pts',(-0.16154811780732,0.0863532198846474,
-0.3991297206437));
#25116=CARTESIAN_POINT('Ctrl Pts',(-0.161124636119803,-0.0871431951720242,
-0.388137670036532));
#25117=CARTESIAN_POINT('Ctrl Pts',(-0.016166963865162,-0.182462532985216,
-0.377145619429364));
#25118=CARTESIAN_POINT('Ctrl Pts',(0.143291190860782,-0.114114530259385,
-0.366153568822197));
#25119=CARTESIAN_POINT('Ctrl Pts',(0.174215754599295,0.0565982325616605,
-0.35516151821503));
#25120=CARTESIAN_POINT('Ctrl Pts',(0.0488656965331514,0.176540319869506,
-0.344169467607861));
#25121=CARTESIAN_POINT('Ctrl Pts',(-0.120317419627598,0.138123660865276,
-0.333177417000694));
#25122=CARTESIAN_POINT('Ctrl Pts',(-0.181574082384246,-0.0241923660424905,
-0.322185366393526));
#25123=CARTESIAN_POINT('Ctrl Pts',(-0.0799559507003814,-0.164807298147092,
-0.311193315786359));
#25124=CARTESIAN_POINT('Ctrl Pts',(0.0933838621769322,-0.157587648721984,
-0.300201265179191));
#25125=CARTESIAN_POINT('Ctrl Pts',(0.182956936375875,-0.00900941659901149,
-0.289209214572024));
#25126=CARTESIAN_POINT('Ctrl Pts',(0.108414826916839,0.14765037535385,-0.278217163964856));
#25127=CARTESIAN_POINT('Ctrl Pts',(-0.0633770392495001,0.17186553164345,
-0.267225113357688));
#25128=CARTESIAN_POINT('Ctrl Pts',(-0.178318731760777,0.0419146652942395,
-0.25623306275052));
#25129=CARTESIAN_POINT('Ctrl Pts',(-0.133305789961508,-0.125634293193532,
-0.245241012143353));
#25130=CARTESIAN_POINT('Ctrl Pts',(0.031284490132526,-0.180487370051941,
-0.234248961536185));
#25131=CARTESIAN_POINT('Ctrl Pts',(0.167812098115434,-0.0734405049249859,
-0.223256910929018));
#25132=CARTESIAN_POINT('Ctrl Pts',(0.15380969315891,0.0994836089306307,
-0.21226486032185));
#25133=CARTESIAN_POINT('Ctrl Pts',(0.00183761696418741,0.183169418595726,
-0.201272809714682));
#25134=CARTESIAN_POINT('Ctrl Pts',(-0.151782791833885,0.102549420661736,
-0.190280759107515));
#25135=CARTESIAN_POINT('Ctrl Pts',(-0.169251783292637,-0.0700589167820705,
-0.179288708500347));
#25136=CARTESIAN_POINT('Ctrl Pts',(-0.0348991934490358,-0.179823450787922,
-0.168296657893179));
#25137=CARTESIAN_POINT('Ctrl Pts',(0.130758243427182,-0.128283368419821,
-0.157304607286012));
#25138=CARTESIAN_POINT('Ctrl Pts',(0.179124036706147,0.0383284300983071,
-0.146312556678844));
#25139=CARTESIAN_POINT('Ctrl Pts',(0.0668118623371123,0.17055986176609,
-0.135320506071676));
#25140=CARTESIAN_POINT('Ctrl Pts',(-0.105429739997846,0.149794915093888,
-0.124328455464509));
#25141=CARTESIAN_POINT('Ctrl Pts',(-0.183102754328823,-0.00533537128298008,
-0.113336404857341));
#25142=CARTESIAN_POINT('Ctrl Pts',(-0.0965231054289514,-0.155685461973447,
-0.102344354250173));
#25143=CARTESIAN_POINT('Ctrl Pts',(0.0766264864264418,-0.166372403162464,
-0.091352303643006));
#25144=CARTESIAN_POINT('Ctrl Pts',(0.181065301238179,-0.0278415620581252,
-0.0803602530358381));
#25145=CARTESIAN_POINT('Ctrl Pts',(0.123039270360697,0.135703326763709,
-0.0693682024286707));
#25146=CARTESIAN_POINT('Ctrl Pts',(-0.0452659821533855,0.177444214884968,
-0.058376151821503));
#25147=CARTESIAN_POINT('Ctrl Pts',(-0.173137980058957,0.0601617876158408,
-0.0473841012143354));
#25148=CARTESIAN_POINT('Ctrl Pts',(-0.145363928230217,-0.111382333108322,
-0.0363920506071676));
#25149=CARTESIAN_POINT('Ctrl Pts',(-0.0404206461299352,-0.158679121552366,
-0.029064016869056));
#25150=CARTESIAN_POINT('Ctrl Pts',(0.0106175386826097,-0.155187210724091,
-0.0254000000000001));
#25151=CARTESIAN_POINT('Ctrl Pts',(-0.0744392439309313,0.151537102412036,
-0.468404938818138));
#25152=CARTESIAN_POINT('Ctrl Pts',(-0.124276976066047,0.12705542076233,
-0.464740921949082));
#25153=CARTESIAN_POINT('Ctrl Pts',(-0.197120047848906,0.0255487894600746,
-0.45741288821097));
#25154=CARTESIAN_POINT('Ctrl Pts',(-0.129898194597202,-0.150683824391059,
-0.446420837603803));
#25155=CARTESIAN_POINT('Ctrl Pts',(0.0540015778247265,-0.191288854737121,
-0.435428786996635));
#25156=CARTESIAN_POINT('Ctrl Pts',(0.189380354575173,-0.0605358223897492,
-0.424436736389467));
#25157=CARTESIAN_POINT('Ctrl Pts',(0.154924182493192,0.124638539332289,
-0.413444685782299));
#25158=CARTESIAN_POINT('Ctrl Pts',(-0.0185234112613053,0.197947604266499,
-0.402452635175133));
#25159=CARTESIAN_POINT('Ctrl Pts',(-0.175343665851082,0.0937274314187808,
-0.391460584567963));
#25160=CARTESIAN_POINT('Ctrl Pts',(-0.174884020560764,-0.0945848673623276,
-0.380468533960798));
#25161=CARTESIAN_POINT('Ctrl Pts',(-0.0175475564078102,-0.1980440864824,
-0.369476483353628));
#25162=CARTESIAN_POINT('Ctrl Pts',(0.155527672068972,-0.123859444072385,
-0.358484432746461));
#25163=CARTESIAN_POINT('Ctrl Pts',(0.189093066976413,0.061431489965672,
-0.347492382139294));
#25164=CARTESIAN_POINT('Ctrl Pts',(0.0530386270096244,0.191616140606247,
-0.336500331532126));
#25165=CARTESIAN_POINT('Ctrl Pts',(-0.130592034804196,0.149918856162568,
-0.325508280924959));
#25166=CARTESIAN_POINT('Ctrl Pts',(-0.197079765836539,-0.0262582950830843,
-0.314516230317791));
#25167=CARTESIAN_POINT('Ctrl Pts',(-0.0867838616302223,-0.178881166852035,
-0.303524179710623));
#25168=CARTESIAN_POINT('Ctrl Pts',(0.101358461786384,-0.171044988916071,
-0.292532129103456));
#25169=CARTESIAN_POINT('Ctrl Pts',(0.198580709899027,-0.0097787839009954,
-0.281540078496288));
#25170=CARTESIAN_POINT('Ctrl Pts',(0.117673009393291,0.160259113075592,
-0.27054802788912));
#25171=CARTESIAN_POINT('Ctrl Pts',(-0.0687891789989752,0.186542144599608,
-0.259555977281953));
#25172=CARTESIAN_POINT('Ctrl Pts',(-0.193546421593985,0.0454940061535037,
-0.248563926674785));
#25173=CARTESIAN_POINT('Ctrl Pts',(-0.14468955880318,-0.13636294761068,
-0.237571876067617));
#25174=CARTESIAN_POINT('Ctrl Pts',(0.0339560575423216,-0.195900252718971,
-0.226579825460449));
#25175=CARTESIAN_POINT('Ctrl Pts',(0.182142564439017,-0.0797120234533494,
-0.215587774853282));
#25176=CARTESIAN_POINT('Ctrl Pts',(0.166944411411096,0.107979101946565,
-0.204595724246114));
#25177=CARTESIAN_POINT('Ctrl Pts',(0.00199454193155687,0.198811337230763,
-0.193603673638947));
#25178=CARTESIAN_POINT('Ctrl Pts',(-0.164744421009028,0.111306721451129,
-0.182611623031779));
#25179=CARTESIAN_POINT('Ctrl Pts',(-0.183705192837717,-0.0760416615238799,
-0.171619572424612));
#25180=CARTESIAN_POINT('Ctrl Pts',(-0.037879441727069,-0.195179637467229,
-0.160627521817444));
#25181=CARTESIAN_POINT('Ctrl Pts',(0.141924462221939,-0.13923824301862,
-0.149635471210276));
#25182=CARTESIAN_POINT('Ctrl Pts',(0.194420496285574,0.0416015211503103,
-0.138643420603109));
#25183=CARTESIAN_POINT('Ctrl Pts',(0.0725173219195277,0.185124975858833,
-0.127651369995941));
#25184=CARTESIAN_POINT('Ctrl Pts',(-0.114433008269386,0.162586787731822,
-0.116659319388773));
#25185=CARTESIAN_POINT('Ctrl Pts',(-0.198738980108323,-0.00579099015285377,
-0.105667268781606));
#25186=CARTESIAN_POINT('Ctrl Pts',(-0.104765783563193,-0.168980363204866,
-0.0946752181744379));
#25187=CARTESIAN_POINT('Ctrl Pts',(0.0831700747347963,-0.180579925429739,
-0.0836831675672704));
#25188=CARTESIAN_POINT('Ctrl Pts',(0.19652753686304,-0.0302191175022836,
-0.0726911169601027));
#25189=CARTESIAN_POINT('Ctrl Pts',(0.133546320449358,0.147291835435162,
-0.0616990663529351));
#25190=CARTESIAN_POINT('Ctrl Pts',(-0.0491315117554692,0.192597224556383,
-0.0507070157457675));
#25191=CARTESIAN_POINT('Ctrl Pts',(-0.187923254901664,0.0652993580358375,
-0.0397149651385998));
#25192=CARTESIAN_POINT('Ctrl Pts',(-0.157777412726036,-0.120893928467513,
-0.0287229145314321));
#25193=CARTESIAN_POINT('Ctrl Pts',(-0.043872403867593,-0.172229669058767,
-0.0213948807933204));
#25194=CARTESIAN_POINT('Ctrl Pts',(0.0115242330284832,-0.168439563338159,
-0.0177308639242646));
#25195=CARTESIAN_POINT('Ctrl Pts',(-0.0802959149489916,0.163459616787395,
-0.460735802742402));
#25196=CARTESIAN_POINT('Ctrl Pts',(-0.134054740125735,0.137051785061202,
-0.457071785873346));
#25197=CARTESIAN_POINT('Ctrl Pts',(-0.212628900576999,0.0275588965873877,
-0.449743752135234));
#25198=CARTESIAN_POINT('Ctrl Pts',(-0.140118220371533,-0.162539205243939,
-0.438751701528067));
#25199=CARTESIAN_POINT('Ctrl Pts',(0.0582502705716468,-0.206338925539242,
-0.427759650920899));
#25200=CARTESIAN_POINT('Ctrl Pts',(0.204280269935135,-0.06529861117994,
-0.416767600313732));
#25201=CARTESIAN_POINT('Ctrl Pts',(0.167113182833476,0.134444750176102,
-0.405775549706564));
#25202=CARTESIAN_POINT('Ctrl Pts',(-0.0199807813279645,0.213521566813429,
-0.394783499099397));
#25203=CARTESIAN_POINT('Ctrl Pts',(-0.189139213894845,0.101101642952914,
-0.383791448492229));
#25204=CARTESIAN_POINT('Ctrl Pts',(-0.188643405001724,-0.102026539552631,
-0.372799397885061));
#25205=CARTESIAN_POINT('Ctrl Pts',(-0.0189281489504585,-0.213625639979584,
-0.361807347277894));
#25206=CARTESIAN_POINT('Ctrl Pts',(0.167764153277162,-0.133604357885385,
-0.350815296670725));
#25207=CARTESIAN_POINT('Ctrl Pts',(0.203970379353531,0.0662647473696836,
-0.339823246063558));
#25208=CARTESIAN_POINT('Ctrl Pts',(0.0572115574860978,0.206691961342987,
-0.328831195456391));
#25209=CARTESIAN_POINT('Ctrl Pts',(-0.140866649980795,0.16171405145986,
-0.317839144849223));
#25210=CARTESIAN_POINT('Ctrl Pts',(-0.212585449288831,-0.0283242241236782,
-0.306847094242055));
#25211=CARTESIAN_POINT('Ctrl Pts',(-0.0936117725600636,-0.192955035556977,
-0.295855043634888));
#25212=CARTESIAN_POINT('Ctrl Pts',(0.109333061395836,-0.18450232911016,
-0.28486299302772));
#25213=CARTESIAN_POINT('Ctrl Pts',(0.214204483422178,-0.0105481512029789,
-0.273870942420553));
#25214=CARTESIAN_POINT('Ctrl Pts',(0.126931191869743,0.172867850797333,
-0.262878891813384));
#25215=CARTESIAN_POINT('Ctrl Pts',(-0.07420131874845,0.201218757555768,
-0.251886841206217));
#25216=CARTESIAN_POINT('Ctrl Pts',(-0.208774111427194,0.0490733470127675,
-0.240894790599049));
#25217=CARTESIAN_POINT('Ctrl Pts',(-0.156073327644852,-0.147091602027827,
-0.229902739991882));
#25218=CARTESIAN_POINT('Ctrl Pts',(0.0366276249521169,-0.211313135386002,
-0.218910689384714));
#25219=CARTESIAN_POINT('Ctrl Pts',(0.1964730307626,-0.0859835419817126,
-0.207918638777546));
#25220=CARTESIAN_POINT('Ctrl Pts',(0.180079129663282,0.116474594962498,
-0.196926588170379));
#25221=CARTESIAN_POINT('Ctrl Pts',(0.00215146689892645,0.214453255865799,
-0.185934537563211));
#25222=CARTESIAN_POINT('Ctrl Pts',(-0.17770605018417,0.120064022240522,
-0.174942486956044));
#25223=CARTESIAN_POINT('Ctrl Pts',(-0.198158602382797,-0.0820244062656893,
-0.163950436348876));
#25224=CARTESIAN_POINT('Ctrl Pts',(-0.0408596900051022,-0.210535824146536,
-0.152958385741708));
#25225=CARTESIAN_POINT('Ctrl Pts',(0.153090681016695,-0.15019311761742,
-0.141966335134541));
#25226=CARTESIAN_POINT('Ctrl Pts',(0.209716955865002,0.0448746122023138,
-0.130974284527373));
#25227=CARTESIAN_POINT('Ctrl Pts',(0.0782227815019429,0.199690089951577,
-0.119982233920205));
#25228=CARTESIAN_POINT('Ctrl Pts',(-0.123436276540926,0.175378660369755,
-0.108990183313038));
#25229=CARTESIAN_POINT('Ctrl Pts',(-0.214375205887822,-0.0062466090227276,
-0.0979981327058702));
#25230=CARTESIAN_POINT('Ctrl Pts',(-0.113008461697435,-0.182275264436286,
-0.0870060820987024));
#25231=CARTESIAN_POINT('Ctrl Pts',(0.0897136630431509,-0.194787447697015,
-0.076014031491535));
#25232=CARTESIAN_POINT('Ctrl Pts',(0.211989772487901,-0.0325966729464418,
-0.0650219808843671));
#25233=CARTESIAN_POINT('Ctrl Pts',(0.14405337053802,0.158880344106616,-0.0540299302771997));
#25234=CARTESIAN_POINT('Ctrl Pts',(-0.0529970413575529,0.207750234227798,
-0.0430378796700319));
#25235=CARTESIAN_POINT('Ctrl Pts',(-0.202708529744371,0.0704369284558339,
-0.0320458290628643));
#25236=CARTESIAN_POINT('Ctrl Pts',(-0.170190897221856,-0.130405523826704,
-0.0210537784556966));
#25237=CARTESIAN_POINT('Ctrl Pts',(-0.0473241616052508,-0.185780216565167,
-0.0137257447175849));
#25238=CARTESIAN_POINT('Ctrl Pts',(0.0124309273743567,-0.181691915952227,
-0.010061727848529));
#25239=CARTESIAN_POINT('Ctrl Pts',(-0.0861525859670518,0.175382131162755,
-0.453066666666667));
#25240=CARTESIAN_POINT('Ctrl Pts',(-0.143832504185423,0.147048149360075,
-0.449402649797611));
#25241=CARTESIAN_POINT('Ctrl Pts',(-0.228137753305091,0.0295690037147008,
-0.442074616059499));
#25242=CARTESIAN_POINT('Ctrl Pts',(-0.150338246145864,-0.174394586096819,
-0.431082565452331));
#25243=CARTESIAN_POINT('Ctrl Pts',(0.0624989633185675,-0.221388996341363,
-0.420090514845164));
#25244=CARTESIAN_POINT('Ctrl Pts',(0.219180185295097,-0.0700613999701309,
-0.409098464237996));
#25245=CARTESIAN_POINT('Ctrl Pts',(0.17930218317376,0.144250961019916,-0.398106413630828));
#25246=CARTESIAN_POINT('Ctrl Pts',(-0.0214381513946237,0.229095529360358,
-0.387114363023661));
#25247=CARTESIAN_POINT('Ctrl Pts',(-0.202934761938607,0.108475854487047,
-0.376122312416493));
#25248=CARTESIAN_POINT('Ctrl Pts',(-0.202402789442685,-0.109468211742934,
-0.365130261809326));
#25249=CARTESIAN_POINT('Ctrl Pts',(-0.0203087414931069,-0.229207193476768,
-0.354138211202158));
#25250=CARTESIAN_POINT('Ctrl Pts',(0.180000634485353,-0.143349271698386,
-0.34314616059499));
#25251=CARTESIAN_POINT('Ctrl Pts',(0.218847691730649,0.0710980047736953,
-0.332154109987823));
#25252=CARTESIAN_POINT('Ctrl Pts',(0.0613844879625708,0.221767782079727,
-0.321162059380655));
#25253=CARTESIAN_POINT('Ctrl Pts',(-0.151141265157393,0.173509246757153,
-0.310170008773488));
#25254=CARTESIAN_POINT('Ctrl Pts',(-0.228091132741123,-0.030390153164272,
-0.29917795816632));
#25255=CARTESIAN_POINT('Ctrl Pts',(-0.100439683489904,-0.20702890426192,
-0.288185907559152));
#25256=CARTESIAN_POINT('Ctrl Pts',(0.117307661005287,-0.197959669304247,
-0.277193856951985));
#25257=CARTESIAN_POINT('Ctrl Pts',(0.22982825694533,-0.011317518504963,
-0.266201806344817));
#25258=CARTESIAN_POINT('Ctrl Pts',(0.136189374346194,0.185476588519076,
-0.255209755737649));
#25259=CARTESIAN_POINT('Ctrl Pts',(-0.0796134584979247,0.215895370511926,
-0.244217705130482));
#25260=CARTESIAN_POINT('Ctrl Pts',(-0.224001801260403,0.0526526878720317,
-0.233225654523314));
#25261=CARTESIAN_POINT('Ctrl Pts',(-0.167457096486523,-0.157820256444976,
-0.222233603916146));
#25262=CARTESIAN_POINT('Ctrl Pts',(0.0392991923619123,-0.226726018053033,
-0.211241553308979));
#25263=CARTESIAN_POINT('Ctrl Pts',(0.210803497086183,-0.0922550605100761,
-0.200249502701811));
#25264=CARTESIAN_POINT('Ctrl Pts',(0.193213847915468,0.124970087978432,
-0.189257452094643));
#25265=CARTESIAN_POINT('Ctrl Pts',(0.00230839186629608,0.230095174500836,
-0.178265401487476));
#25266=CARTESIAN_POINT('Ctrl Pts',(-0.190667679359313,0.128821323029915,
-0.167273350880308));
#25267=CARTESIAN_POINT('Ctrl Pts',(-0.212612011927877,-0.0880071510074988,
-0.15628130027314));
#25268=CARTESIAN_POINT('Ctrl Pts',(-0.0438399382831356,-0.225892010825843,
-0.145289249665973));
#25269=CARTESIAN_POINT('Ctrl Pts',(0.164256899811452,-0.16114799221622,
-0.134297199058805));
#25270=CARTESIAN_POINT('Ctrl Pts',(0.22501341544443,0.0481477032543172,
-0.123305148451638));
#25271=CARTESIAN_POINT('Ctrl Pts',(0.0839282410843581,0.21425520404432,
-0.11231309784447));
#25272=CARTESIAN_POINT('Ctrl Pts',(-0.132439544812465,0.188170533007688,
-0.101321047237302));
#25273=CARTESIAN_POINT('Ctrl Pts',(-0.230011431667322,-0.00670222789260128,
-0.0903289966301345));
#25274=CARTESIAN_POINT('Ctrl Pts',(-0.121251139831676,-0.195570165667705,
-0.079336946022967));
#25275=CARTESIAN_POINT('Ctrl Pts',(0.0962572513515054,-0.208994969964291,
-0.0683448954157993));
#25276=CARTESIAN_POINT('Ctrl Pts',(0.227452008112762,-0.0349742283906001,
-0.0573528448086317));
#25277=CARTESIAN_POINT('Ctrl Pts',(0.154560420626681,0.170468852778069,
-0.0463607942014641));
#25278=CARTESIAN_POINT('Ctrl Pts',(-0.0568625709596362,0.222903243899213,
-0.0353687435942964));
#25279=CARTESIAN_POINT('Ctrl Pts',(-0.217493804587078,0.0755744988758305,
-0.0243766929871288));
#25280=CARTESIAN_POINT('Ctrl Pts',(-0.182604381717675,-0.139917119185895,
-0.0133846423799611));
#25281=CARTESIAN_POINT('Ctrl Pts',(-0.0507759193429087,-0.199330764071568,
-0.00605660864184936));
#25282=CARTESIAN_POINT('Ctrl Pts',(0.0133376217202303,-0.194944268566296,
-0.0023925917727935));
#25283=CARTESIAN_POINT('Ctrl Pts',(-0.195698342875023,-3.28562868159645E-5,
-0.0906536358790898));
#25284=CARTESIAN_POINT('Ctrl Pts',(-0.195702885553977,-0.00192275150872445,
-0.0905454227961047));
#25285=CARTESIAN_POINT('Ctrl Pts',(-0.195677808282155,-0.0038125242527969,
-0.0904372097131196));
#25286=CARTESIAN_POINT('Ctrl Pts',(-0.195622735218905,-0.00570142403840418,
-0.0903289966301345));
#25287=CARTESIAN_POINT('Ctrl Pts',(-0.19375800105544,-0.0696582071509693,
-0.0866649797610786));
#25288=CARTESIAN_POINT('Ctrl Pts',(-0.157504570443558,-0.132614186409337,
-0.0830009628920228));
#25289=CARTESIAN_POINT('Ctrl Pts',(-0.103126456607088,-0.166329643421285,
-0.079336946022967));
#25290=CARTESIAN_POINT('Ctrl Pts',(-0.0487483427706158,-0.200045100433234,
-0.0756729291539111));
#25291=CARTESIAN_POINT('Ctrl Pts',(0.0237544542904457,-0.204520035198762,
-0.0720089122848551));
#25292=CARTESIAN_POINT('Ctrl Pts',(0.0818716456145191,-0.177754045652577,
-0.0683448954157992));
#25293=CARTESIAN_POINT('Ctrl Pts',(0.139988836938592,-0.150988056106393,
-0.0646808785467433));
#25294=CARTESIAN_POINT('Ctrl Pts',(0.183720422525678,-0.0929811422484953,
-0.0610168616776875));
#25295=CARTESIAN_POINT('Ctrl Pts',(0.193437617404873,-0.0297371717914351,
-0.0573528448086316));
#25296=CARTESIAN_POINT('Ctrl Pts',(0.203154812284068,0.0335067986656242,
-0.0536888279395758));
#25297=CARTESIAN_POINT('Ctrl Pts',(0.178857616455375,0.101987825721846,
-0.0500248110705199));
#25298=CARTESIAN_POINT('Ctrl Pts',(0.131471853276642,0.144967404436815,
-0.0463607942014641));
#25299=CARTESIAN_POINT('Ctrl Pts',(0.084086090097909,0.187946983151784,
-0.0426967773324082));
#25300=CARTESIAN_POINT('Ctrl Pts',(0.0136117595691364,0.205425113525499,
-0.0390327604633523));
#25301=CARTESIAN_POINT('Ctrl Pts',(-0.0483972779664903,0.189609387875126,
-0.0353687435942964));
#25302=CARTESIAN_POINT('Ctrl Pts',(-0.104633572522728,0.175266030170468,
-0.0320458290628643));
#25303=CARTESIAN_POINT('Ctrl Pts',(-0.153907363890767,0.133539263657296,
-0.0287229145314322));
#25304=CARTESIAN_POINT('Ctrl Pts',(-0.178226250896966,0.0807893643570689,
-0.0254000000000001));
#25305=CARTESIAN_POINT('',(-0.0903606778650201,-0.126612599672284,-0.453066666666667));
#25306=CARTESIAN_POINT('Ctrl Pts',(-0.0905470291188205,-0.126755563903434,
-0.453066666666667));
#25307=CARTESIAN_POINT('Ctrl Pts',(-0.0947991957642303,-0.124487575468212,
-0.453066666666667));
#25308=CARTESIAN_POINT('Ctrl Pts',(-0.0989294677700178,-0.122016794807246,
-0.453066666666667));
#25309=CARTESIAN_POINT('Ctrl Pts',(-0.10292135951426,-0.119346893969649,
-0.453066666666667));
#25310=CARTESIAN_POINT('Ctrl Pts',(-0.108133628568249,-0.115860766989102,
-0.453066666666667));
#25311=CARTESIAN_POINT('Ctrl Pts',(-0.113110147998552,-0.112035408131854,
-0.453066666666667));
#25312=CARTESIAN_POINT('Ctrl Pts',(-0.117841914883643,-0.107907652239557,
-0.453066666666667));
#25313=CARTESIAN_POINT('Ctrl Pts',(-0.122114349501896,-0.104180594758025,
-0.453066666666667));
#25314=CARTESIAN_POINT('Ctrl Pts',(-0.126190272687336,-0.100202764591398,
-0.453066666666667));
#25315=CARTESIAN_POINT('Ctrl Pts',(-0.130041327864726,-0.0960214698833582,
-0.453066666666667));
#25316=CARTESIAN_POINT('Ctrl Pts',(-0.135935559478366,-0.089621790232241,
-0.453066666666667));
#25317=CARTESIAN_POINT('Ctrl Pts',(-0.141313195335496,-0.0827394474627572,
-0.453066666666667));
#25318=CARTESIAN_POINT('Ctrl Pts',(-0.146148572761508,-0.0754634735042225,
-0.453066666666667));
#25319=CARTESIAN_POINT('Ctrl Pts',(-0.149168330159111,-0.0709195311704024,
-0.453066666666667));
#25320=CARTESIAN_POINT('Ctrl Pts',(-0.151978671030338,-0.0662164416771034,
-0.453066666666667));
#25321=CARTESIAN_POINT('Ctrl Pts',(-0.154556741894587,-0.0614028695358839,
-0.453066666666667));
#25322=CARTESIAN_POINT('Ctrl Pts',(-0.160075954266155,-0.0510978281649633,
-0.453066666666667));
#25323=CARTESIAN_POINT('Ctrl Pts',(-0.164547838171259,-0.040270898794287,
-0.453066666666667));
#25324=CARTESIAN_POINT('Ctrl Pts',(-0.167909402584567,-0.0291166800107643,
-0.453066666666667));
#25325=CARTESIAN_POINT('Ctrl Pts',(-0.169458518128482,-0.0239764620725413,
-0.453066666666667));
#25326=CARTESIAN_POINT('Ctrl Pts',(-0.17077135633224,-0.0187661737549059,
-0.453066666666667));
#25327=CARTESIAN_POINT('Ctrl Pts',(-0.171838785035581,-0.0135026857692308,
-0.453066666666667));
#25328=CARTESIAN_POINT('Ctrl Pts',(-0.172761838697209,-0.00895111071517557,
-0.453066666666667));
#25329=CARTESIAN_POINT('Ctrl Pts',(-0.173501415363079,-0.00435555596891192,
-0.453066666666667));
#25330=CARTESIAN_POINT('Ctrl Pts',(-0.174048163489164,0.000245370197640356,
-0.453066666666667));
#25331=CARTESIAN_POINT('Ctrl Pts',(-0.174928992407005,0.00765761108701054,
-0.453066666666667));
#25332=CARTESIAN_POINT('Ctrl Pts',(-0.175313137595295,0.0150962164885127,
-0.453066666666667));
#25333=CARTESIAN_POINT('Ctrl Pts',(-0.17518323296547,0.0225143573359635,
-0.453066666666667));
#25334=CARTESIAN_POINT('Ctrl Pts',(-0.175047559449211,0.0302619276437026,
-0.453066666666667));
#25335=CARTESIAN_POINT('Ctrl Pts',(-0.174351423432551,0.0379873668160185,
-0.453066666666667));
#25336=CARTESIAN_POINT('Ctrl Pts',(-0.173130401268424,0.0456510136887945,
-0.453066666666667));
#25337=CARTESIAN_POINT('Ctrl Pts',(-0.172378019222284,0.0503732787585368,
-0.453066666666667));
#25338=CARTESIAN_POINT('Ctrl Pts',(-0.171426132330918,0.0550721261644083,
-0.453066666666667));
#25339=CARTESIAN_POINT('Ctrl Pts',(-0.170281162641598,0.0597383409928608,
-0.453066666666667));
#25340=CARTESIAN_POINT('Ctrl Pts',(-0.169381700085032,0.0634040149039102,
-0.453066666666667));
#25341=CARTESIAN_POINT('Ctrl Pts',(-0.168364960525766,0.0670413292940973,
-0.453066666666667));
#25342=CARTESIAN_POINT('Ctrl Pts',(-0.167236908480682,0.0706411471149374,
-0.453066666666667));
#25343=CARTESIAN_POINT('Ctrl Pts',(-0.163878286349993,0.0813591169570331,
-0.453066666666667));
#25344=CARTESIAN_POINT('Ctrl Pts',(-0.159532509087918,0.0917579355296217,
-0.453066666666667));
#25345=CARTESIAN_POINT('Ctrl Pts',(-0.154300403897806,0.101723195040055,
-0.453066666666667));
#25346=CARTESIAN_POINT('Ctrl Pts',(-0.150458279880649,0.109041045410227,
-0.453066666666667));
#25347=CARTESIAN_POINT('Ctrl Pts',(-0.146137323639187,0.11612533476953,
-0.453066666666667));
#25348=CARTESIAN_POINT('Ctrl Pts',(-0.141365363239444,0.122928507327059,
-0.453066666666667));
#25349=CARTESIAN_POINT('Ctrl Pts',(-0.139474935210954,0.12562360682665,
-0.453066666666667));
#25350=CARTESIAN_POINT('Ctrl Pts',(-0.137514595596603,0.128272882481353,
-0.453066666666667));
#25351=CARTESIAN_POINT('Ctrl Pts',(-0.13549208476146,0.130866201634327,
-0.453066666666667));
#25352=CARTESIAN_POINT('Ctrl Pts',(-0.127604957338041,0.140979293862904,
-0.453066666666667));
#25353=CARTESIAN_POINT('Ctrl Pts',(-0.118753988352663,0.150274988313495,
-0.453066666666667));
#25354=CARTESIAN_POINT('Ctrl Pts',(-0.109058348041544,0.1585911082717,-0.453066666666667));
#25355=CARTESIAN_POINT('Ctrl Pts',(-0.101876675688201,0.164750954024479,
-0.453066666666667));
#25356=CARTESIAN_POINT('Ctrl Pts',(-0.0942303837916874,0.17037340113684,
-0.453066666666667));
#25357=CARTESIAN_POINT('Ctrl Pts',(-0.0861525859670518,0.175382131162755,
-0.453066666666667));
#25358=CARTESIAN_POINT('Ctrl Pts',(-0.0905470291188203,-0.126755563903435,
-0.453066666666667));
#25359=CARTESIAN_POINT('Ctrl Pts',(-0.0527502457699392,-0.153392327621369,
-0.449743752135235));
#25360=CARTESIAN_POINT('Ctrl Pts',(0.0536233967596413,-0.172500523394585,
-0.442756820734747));
#25361=CARTESIAN_POINT('Ctrl Pts',(0.174480439215212,-0.0557730335995584,
-0.432105872465203));
#25362=CARTESIAN_POINT('Ctrl Pts',(0.142735182152908,0.114832328488475,
-0.421113821858035));
#25363=CARTESIAN_POINT('Ctrl Pts',(-0.017066041194646,0.182373641719569,
-0.410121771250868));
#25364=CARTESIAN_POINT('Ctrl Pts',(-0.137347945518334,0.102436258045122,
-0.400970845333621));
#25365=CARTESIAN_POINT('Ctrl Pts',(-0.155309689873578,0.0255484863100586,
-0.395483936285431));
#25366=CARTESIAN_POINT('Ctrl Pts',(-0.155306872404023,2.87756186839044E-6,
-0.393661044106296));
#25367=CARTESIAN_POINT('Origin',(-2.59090492670967E-17,0.,-0.453066666666667));
#25368=CARTESIAN_POINT('',(-0.1954,-2.39295984553393E-17,-0.453066666666667));
#25369=CARTESIAN_POINT('Origin',(0.,0.,-0.453066666666667));
#25370=CARTESIAN_POINT('Origin',(0.,0.,-0.453066666666667));
#25371=CARTESIAN_POINT('',(0.0903606778650194,-0.126612599672285,-0.453066666666667));
#25372=CARTESIAN_POINT('Ctrl Pts',(0.0863544310469494,0.175597323663767,
-0.453066666666667));
#25373=CARTESIAN_POINT('Ctrl Pts',(0.0914440695611803,0.172479495245472,
-0.453066666666667));
#25374=CARTESIAN_POINT('Ctrl Pts',(0.096371458315283,0.169121306427088,
-0.453066666666667));
#25375=CARTESIAN_POINT('Ctrl Pts',(0.10111644025993,0.165522169603453,-0.453066666666667));
#25376=CARTESIAN_POINT('Ctrl Pts',(0.108664242830105,0.159797053157331,
-0.453066666666667));
#25377=CARTESIAN_POINT('Ctrl Pts',(0.115751223714214,0.15346251089447,-0.453066666666667));
#25378=CARTESIAN_POINT('Ctrl Pts',(0.122338307079031,0.146595406424471,
-0.453066666666667));
#25379=CARTESIAN_POINT('Ctrl Pts',(0.125481640567847,0.143318447828952,
-0.453066666666667));
#25380=CARTESIAN_POINT('Ctrl Pts',(0.128510764277807,0.139919788637431,
-0.453066666666667));
#25381=CARTESIAN_POINT('Ctrl Pts',(0.131411861578166,0.136419098604737,
-0.453066666666667));
#25382=CARTESIAN_POINT('Ctrl Pts',(0.135978580737029,0.130908539465763,
-0.453066666666667));
#25383=CARTESIAN_POINT('Ctrl Pts',(0.140234769092733,0.125138834436613,
-0.453066666666667));
#25384=CARTESIAN_POINT('Ctrl Pts',(0.144163533941065,0.119143612028972,
-0.453066666666667));
#25385=CARTESIAN_POINT('Ctrl Pts',(0.146833444162397,0.115069378471289,
-0.453066666666667));
#25386=CARTESIAN_POINT('Ctrl Pts',(0.149352043837122,0.110890938917105,
-0.453066666666667));
#25387=CARTESIAN_POINT('Ctrl Pts',(0.151712670729972,0.106618527140408,
-0.453066666666667));
#25388=CARTESIAN_POINT('Ctrl Pts',(0.153749069602213,0.102932923731346,
-0.453066666666667));
#25389=CARTESIAN_POINT('Ctrl Pts',(0.155668099628493,0.0991762472086667,
-0.453066666666667));
#25390=CARTESIAN_POINT('Ctrl Pts',(0.157458355919879,0.0953708013500012,
-0.453066666666667));
#25391=CARTESIAN_POINT('Ctrl Pts',(0.162674643606049,0.0842828356389133,
-0.453066666666667));
#25392=CARTESIAN_POINT('Ctrl Pts',(0.166818779325598,0.0727518602714819,
-0.453066666666667));
#25393=CARTESIAN_POINT('Ctrl Pts',(0.169793416329498,0.0609460732476128,
-0.453066666666667));
#25394=CARTESIAN_POINT('Ctrl Pts',(0.171274420410269,0.0550682405116701,
-0.453066666666667));
#25395=CARTESIAN_POINT('Ctrl Pts',(0.172464744273862,0.0491221862213701,
-0.453066666666667));
#25396=CARTESIAN_POINT('Ctrl Pts',(0.173347398641795,0.0431291460428445,
-0.453066666666667));
#25397=CARTESIAN_POINT('Ctrl Pts',(0.17408748866872,0.038104088185292,-0.453066666666667));
#25398=CARTESIAN_POINT('Ctrl Pts',(0.174611083947877,0.0330404757442079,
-0.453066666666667));
#25399=CARTESIAN_POINT('Ctrl Pts',(0.174905738682316,0.0279831639491109,
-0.453066666666667));
#25400=CARTESIAN_POINT('Ctrl Pts',(0.175329793223554,0.0207048962598366,
-0.453066666666667));
#25401=CARTESIAN_POINT('Ctrl Pts',(0.175282645291204,0.0134289205807883,
-0.453066666666667));
#25402=CARTESIAN_POINT('Ctrl Pts',(0.17473922538412,0.00619266267667447,
-0.453066666666667));
#25403=CARTESIAN_POINT('Ctrl Pts',(0.174114861056575,-0.00212146281144542,
-0.453066666666667));
#25404=CARTESIAN_POINT('Ctrl Pts',(0.172835412310392,-0.0103834978381202,
-0.453066666666667));
#25405=CARTESIAN_POINT('Ctrl Pts',(0.170934029955228,-0.0185322403951933,
-0.453066666666667));
#25406=CARTESIAN_POINT('Ctrl Pts',(0.170056634189217,-0.0222924899833254,
-0.453066666666667));
#25407=CARTESIAN_POINT('Ctrl Pts',(0.169046648886972,-0.026028521993633,
-0.453066666666667));
#25408=CARTESIAN_POINT('Ctrl Pts',(0.167906623664754,-0.0297337195488689,
-0.453066666666667));
#25409=CARTESIAN_POINT('Ctrl Pts',(0.166809883321851,-0.0332982368578347,
-0.453066666666667));
#25410=CARTESIAN_POINT('Ctrl Pts',(0.165594849559875,-0.03682704705354,
-0.453066666666667));
#25411=CARTESIAN_POINT('Ctrl Pts',(0.164267500928256,-0.040308558913606,
-0.453066666666667));
#25412=CARTESIAN_POINT('Ctrl Pts',(0.160821937353092,-0.0493459513256594,
-0.453066666666667));
#25413=CARTESIAN_POINT('Ctrl Pts',(0.15661671770766,-0.0580797720896872,
-0.453066666666667));
#25414=CARTESIAN_POINT('Ctrl Pts',(0.151706204031545,-0.0664127300959662,
-0.453066666666667));
#25415=CARTESIAN_POINT('Ctrl Pts',(0.148524313608442,-0.0718122791095982,
-0.453066666666667));
#25416=CARTESIAN_POINT('Ctrl Pts',(0.145045835105011,-0.0770432405818312,
-0.453066666666667));
#25417=CARTESIAN_POINT('Ctrl Pts',(0.141281936888369,-0.0820744584948006,
-0.453066666666667));
#25418=CARTESIAN_POINT('Ctrl Pts',(0.138548339780333,-0.0857284687642547,
-0.453066666666667));
#25419=CARTESIAN_POINT('Ctrl Pts',(0.135660987987668,-0.0892799913913371,
-0.453066666666667));
#25420=CARTESIAN_POINT('Ctrl Pts',(0.132642788533104,-0.092695561292154,
-0.453066666666667));
#25421=CARTESIAN_POINT('Ctrl Pts',(0.125505940850058,-0.100772032877247,
-0.453066666666667));
#25422=CARTESIAN_POINT('Ctrl Pts',(0.117623386795444,-0.108115570666922,
-0.453066666666667));
#25423=CARTESIAN_POINT('Ctrl Pts',(0.109060973524496,-0.114571708227664,
-0.453066666666667));
#25424=CARTESIAN_POINT('Ctrl Pts',(0.103146709058551,-0.119031117479996,
-0.453066666666667));
#25425=CARTESIAN_POINT('Ctrl Pts',(0.096907460496945,-0.123066412220614,
-0.453066666666667));
#25426=CARTESIAN_POINT('Ctrl Pts',(0.0903606778650195,-0.126612599672284,
-0.453066666666667));
#25427=CARTESIAN_POINT('Origin',(0.,0.,-0.453066666666667));
#25428=CARTESIAN_POINT('Origin',(0.,0.,-0.582472289227037));
#25429=CARTESIAN_POINT('Ctrl Pts',(0.0903606778650195,-0.126612599672284,
-0.453066666666667));
#25430=CARTESIAN_POINT('Ctrl Pts',(0.13200120501619,-0.0968946547775781,
-0.449402649797611));
#25431=CARTESIAN_POINT('Ctrl Pts',(0.183022071105112,0.00628961186891934,
-0.442074616059498));
#25432=CARTESIAN_POINT('Ctrl Pts',(0.0955251259476364,0.156432482487892,
-0.431082565452332));
#25433=CARTESIAN_POINT('Ctrl Pts',(-0.0777334665521386,0.165810192362521,
-0.420090514845164));
#25434=CARTESIAN_POINT('Ctrl Pts',(-0.15183132427248,0.0661923464710166,
-0.412220422770065));
#25435=CARTESIAN_POINT('Ctrl Pts',(-0.155733436132797,0.00767225655067851,
-0.408014347564023));
#25436=CARTESIAN_POINT('Ctrl Pts',(-0.155671978531511,0.000121856215612291,
-0.407472289227037));
#25437=CARTESIAN_POINT('Ctrl Pts',(0.113509973994373,-0.159049193030951,
-0.476074074893873));
#25438=CARTESIAN_POINT('Ctrl Pts',(0.165818292897225,-0.121717875561163,
-0.472410058024817));
#25439=CARTESIAN_POINT('Ctrl Pts',(0.229910078392407,0.00790093319952896,
-0.465082024286706));
#25440=CARTESIAN_POINT('Ctrl Pts',(0.119997490261448,0.196508563665278,
-0.454089973679538));
#25441=CARTESIAN_POINT('Ctrl Pts',(-0.0976478261927854,0.208288727660795,
-0.443097923072371));
#25442=CARTESIAN_POINT('Ctrl Pts',(-0.227652540681624,0.033509185963427,
-0.432105872465202));
#25443=CARTESIAN_POINT('Ctrl Pts',(-0.153475136057457,-0.171473007722053,
-0.421113821858035));
#25444=CARTESIAN_POINT('Ctrl Pts',(0.058385281197714,-0.222565815265022,
-0.410121771250867));
#25445=CARTESIAN_POINT('Ctrl Pts',(0.217866153667128,-0.0740531899532077,
-0.3991297206437));
#25446=CARTESIAN_POINT('Ctrl Pts',(0.181921442653058,0.140906976839248,
-0.388137670036532));
#25447=CARTESIAN_POINT('Ctrl Pts',(-0.0172115249937917,0.229460586201424,
-0.377145619429364));
#25448=CARTESIAN_POINT('Ctrl Pts',(-0.200904477330819,0.112190212191809,
-0.366153568822197));
#25449=CARTESIAN_POINT('Ctrl Pts',(-0.204383566249596,-0.105719475415542,
-0.35516151821503));
#25450=CARTESIAN_POINT('Ctrl Pts',(-0.0245271865868318,-0.228795615786734,
-0.344169467607861));
#25451=CARTESIAN_POINT('Ctrl Pts',(0.17733030957008,-0.146639399315481,
-0.333177417000694));
#25452=CARTESIAN_POINT('Ctrl Pts',(0.220119877306813,0.0670550326110528,
-0.322185366393526));
#25453=CARTESIAN_POINT('Ctrl Pts',(0.0654585025290842,0.220599848939463,
-0.311193315786359));
#25454=CARTESIAN_POINT('Ctrl Pts',(-0.147920131106237,0.176263338113089,
-0.300201265179191));
#25455=CARTESIAN_POINT('Ctrl Pts',(-0.228612151540578,-0.0261841492109524,
-0.289209214572024));
#25456=CARTESIAN_POINT('Ctrl Pts',(-0.104235563843226,-0.205144021139667,
-0.278217163964855));
#25457=CARTESIAN_POINT('Ctrl Pts',(0.113641919270494,-0.200086580128886,
-0.267225113357689));
#25458=CARTESIAN_POINT('Ctrl Pts',(0.229580860068318,-0.0155484015533772,
-0.25623306275052));
#25459=CARTESIAN_POINT('Ctrl Pts',(0.139582253066502,0.182936925549361,
-0.245241012143353));
#25460=CARTESIAN_POINT('Ctrl Pts',(-0.0756237771828058,0.217325032354213,
-0.234248961536185));
#25461=CARTESIAN_POINT('Ctrl Pts',(-0.222994113150184,0.0567692494175366,
-0.223256910929018));
#25462=CARTESIAN_POINT('Ctrl Pts',(-0.170335327486915,-0.154709410547125,
-0.21226486032185));
#25463=CARTESIAN_POINT('Ctrl Pts',(0.0351168847121239,-0.227411376050915,
-0.201272809714682));
#25464=CARTESIAN_POINT('Ctrl Pts',(0.209068659861852,-0.0961218204625421,
-0.190280759107515));
#25465=CARTESIAN_POINT('Ctrl Pts',(0.195482745804626,0.121390419213048,
-0.179288708500347));
#25466=CARTESIAN_POINT('Ctrl Pts',(0.00654561884687529,0.230013710456001,
-0.168296657893179));
#25467=CARTESIAN_POINT('Ctrl Pts',(-0.188262656682081,0.132310954890747,
-0.157304607286012));
#25468=CARTESIAN_POINT('Ctrl Pts',(-0.214197154491775,-0.084076326291454,
-0.146312556678844));
#25469=CARTESIAN_POINT('Ctrl Pts',(-0.0479921676516633,-0.225046671975632,
-0.135320506071676));
#25470=CARTESIAN_POINT('Ctrl Pts',(0.161259941744669,-0.164145144311427,
-0.124328455464509));
#25471=CARTESIAN_POINT('Ctrl Pts',(0.225864351711379,0.0439941137533673,
-0.113336404857341));
#25472=CARTESIAN_POINT('Ctrl Pts',(0.0878555482932161,0.21267566501613,
-0.102344354250174));
#25473=CARTESIAN_POINT('Ctrl Pts',(-0.128943026450155,0.190573028298851,
-0.0913523036430059));
#25474=CARTESIAN_POINT('Ctrl Pts',(-0.23011210049696,-0.00245580332655646,
-0.0803602530358383));
#25475=CARTESIAN_POINT('Ctrl Pts',(-0.124801453245953,-0.193321344114994,
-0.0693682024286707));
#25476=CARTESIAN_POINT('Ctrl Pts',(0.0923324593003295,-0.21069885854053,
-0.058376151821503));
#25477=CARTESIAN_POINT('Ctrl Pts',(0.226884502025437,-0.0392229015181954,
-0.0473841012143354));
#25478=CARTESIAN_POINT('Ctrl Pts',(0.157437865274698,0.167733084004237,
-0.0363920506071677));
#25479=CARTESIAN_POINT('Ctrl Pts',(0.0177060669358754,0.204932776012367,
-0.029064016869056));
#25480=CARTESIAN_POINT('Ctrl Pts',(-0.044842238767986,0.190184998415424,
-0.0254000000000001));
#25481=CARTESIAN_POINT('Ctrl Pts',(0.105793541951255,-0.148236995244729,
-0.468404938818138));
#25482=CARTESIAN_POINT('Ctrl Pts',(0.154545930270213,-0.113443468633301,
-0.464740921949082));
#25483=CARTESIAN_POINT('Ctrl Pts',(0.214280742629976,0.0073638260893257,
-0.457412888210969));
#25484=CARTESIAN_POINT('Ctrl Pts',(0.111840035490177,0.183149869939482,
-0.446420837603803));
#25485=CARTESIAN_POINT('Ctrl Pts',(-0.0910097063125696,0.194129215894703,
-0.435428786996635));
#25486=CARTESIAN_POINT('Ctrl Pts',(-0.212176672810313,0.0312312244133713,
-0.424436736389467));
#25487=CARTESIAN_POINT('Ctrl Pts',(-0.143041863843383,-0.159816236385096,
-0.413444685782299));
#25488=CARTESIAN_POINT('Ctrl Pts',(0.0544162374315441,-0.207435744063536,
-0.402452635175132));
#25489=CARTESIAN_POINT('Ctrl Pts',(0.203055566455196,-0.0690190384355763,
-0.391460584567964));
#25490=CARTESIAN_POINT('Ctrl Pts',(0.169554384499314,0.131328090747395,
-0.380468533960797));
#25491=CARTESIAN_POINT('Ctrl Pts',(-0.0160414818839274,0.213861807013218,
-0.369476483353629));
#25492=CARTESIAN_POINT('Ctrl Pts',(-0.187246948464164,0.104563497835201,
-0.358484432746461));
#25493=CARTESIAN_POINT('Ctrl Pts',(-0.190489528182304,-0.0985326431137525,
-0.347492382139294));
#25494=CARTESIAN_POINT('Ctrl Pts',(-0.0228598232543762,-0.213242041427981,
-0.336500331532126));
#25495=CARTESIAN_POINT('Ctrl Pts',(0.165275357614488,-0.136670821931104,
-0.325508280924959));
#25496=CARTESIAN_POINT('Ctrl Pts',(0.20515608148512,0.0624966173098753,
-0.314516230317791));
#25497=CARTESIAN_POINT('Ctrl Pts',(0.0610086196805955,0.205603424544653,
-0.303524179710623));
#25498=CARTESIAN_POINT('Ctrl Pts',(-0.137864489303809,0.164280919102842,
-0.292532129103455));
#25499=CARTESIAN_POINT('Ctrl Pts',(-0.213071049120087,-0.0244041452088094,
-0.281540078496289));
#25500=CARTESIAN_POINT('Ctrl Pts',(-0.0971496081640168,-0.191198287188087,
-0.27054802788912));
#25501=CARTESIAN_POINT('Ctrl Pts',(0.105916517559595,-0.18648465208703,
-0.259555977281953));
#25502=CARTESIAN_POINT('Ctrl Pts',(0.213973904637198,-0.0144914179267953,
-0.248563926674785));
#25503=CARTESIAN_POINT('Ctrl Pts',(0.130093421976942,0.17050083465352,-0.237571876067617));
#25504=CARTESIAN_POINT('Ctrl Pts',(-0.0704828568130779,0.202551230683597,
-0.22657982546045));
#25505=CARTESIAN_POINT('Ctrl Pts',(-0.207834926167865,0.0529100638336251,
-0.215587774853282));
#25506=CARTESIAN_POINT('Ctrl Pts',(-0.158755895893,-0.144192232092156,-0.204595724246115));
#25507=CARTESIAN_POINT('Ctrl Pts',(0.0327296314610529,-0.211951902602213,
-0.193603673638947));
#25508=CARTESIAN_POINT('Ctrl Pts',(0.194856128139752,-0.089587438774667,
-0.182611623031779));
#25509=CARTESIAN_POINT('Ctrl Pts',(0.182193787393991,0.113138272836999,
-0.171619572424612));
#25510=CARTESIAN_POINT('Ctrl Pts',(0.00610064629305708,0.214377329763965,
-0.160627521817444));
#25511=CARTESIAN_POINT('Ctrl Pts',(-0.175464521457276,0.123316428189286,
-0.149635471210276));
#25512=CARTESIAN_POINT('Ctrl Pts',(-0.199635986619893,-0.0783607998453362,
-0.138643420603109));
#25513=CARTESIAN_POINT('Ctrl Pts',(-0.0447296499428285,-0.209747951610178,
-0.127651369995941));
#25514=CARTESIAN_POINT('Ctrl Pts',(0.150297456793245,-0.152986522679202,
-0.116659319388773));
#25515=CARTESIAN_POINT('Ctrl Pts',(0.210510045304524,0.0410033845942554,
-0.105667268781606));
#25516=CARTESIAN_POINT('Ctrl Pts',(0.0818831095359919,0.198217928320646,
-0.094675218174438));
#25517=CARTESIAN_POINT('Ctrl Pts',(-0.120177452236511,0.177617833522821,
-0.0836831675672705));
#25518=CARTESIAN_POINT('Ctrl Pts',(-0.214469031229127,-0.00228885729693681,
-0.0726911169601027));
#25519=CARTESIAN_POINT('Ctrl Pts',(-0.116317424054805,-0.180179318248426,
-0.0616990663529351));
#25520=CARTESIAN_POINT('Ctrl Pts',(0.0860556791858326,-0.196375505567415,
-0.0507070157457676));
#25521=CARTESIAN_POINT('Ctrl Pts',(0.211460845584438,-0.0365565203760934,
-0.0397149651385997));
#25522=CARTESIAN_POINT('Ctrl Pts',(0.146735205890193,0.156330553472731,
-0.0287229145314322));
#25523=CARTESIAN_POINT('Ctrl Pts',(0.0165024047601763,0.191001402549226,
-0.0213948807933204));
#25524=CARTESIAN_POINT('Ctrl Pts',(-0.0417938538909745,0.17725618199295,
-0.0177308639242646));
#25525=CARTESIAN_POINT('Ctrl Pts',(0.0980771099081373,-0.137424797458507,
-0.460735802742402));
#25526=CARTESIAN_POINT('Ctrl Pts',(0.143273567643201,-0.10516906170544,
-0.457071785873346));
#25527=CARTESIAN_POINT('Ctrl Pts',(0.198651406867544,0.00682671897912246,
-0.449743752135235));
#25528=CARTESIAN_POINT('Ctrl Pts',(0.103682580718907,0.169791176213687,
-0.438751701528067));
#25529=CARTESIAN_POINT('Ctrl Pts',(-0.0843715864323541,0.179969704128612,
-0.427759650920899));
#25530=CARTESIAN_POINT('Ctrl Pts',(-0.196700804939001,0.0289532628633155,
-0.416767600313732));
#25531=CARTESIAN_POINT('Ctrl Pts',(-0.13260859162931,-0.14815946504814,
-0.405775549706564));
#25532=CARTESIAN_POINT('Ctrl Pts',(0.0504471936653742,-0.19230567286205,
-0.394783499099397));
#25533=CARTESIAN_POINT('Ctrl Pts',(0.188244979243263,-0.0639848869179451,
-0.383791448492229));
#25534=CARTESIAN_POINT('Ctrl Pts',(0.157187326345571,0.121749204655543,
-0.372799397885061));
#25535=CARTESIAN_POINT('Ctrl Pts',(-0.014871438774063,0.198263027825011,
-0.361807347277894));
#25536=CARTESIAN_POINT('Ctrl Pts',(-0.17358941959751,0.0969367834785928,
-0.350815296670726));
#25537=CARTESIAN_POINT('Ctrl Pts',(-0.176595490115013,-0.0913458108119624,
-0.339823246063559));
#25538=CARTESIAN_POINT('Ctrl Pts',(-0.021192459921921,-0.197688467069228,
-0.328831195456391));
#25539=CARTESIAN_POINT('Ctrl Pts',(0.153220405658898,-0.126702244546726,
-0.317839144849223));
#25540=CARTESIAN_POINT('Ctrl Pts',(0.190192285663426,0.0579382020086975,
-0.306847094242056));
#25541=CARTESIAN_POINT('Ctrl Pts',(0.056558736832107,0.190607000149843,
-0.295855043634888));
#25542=CARTESIAN_POINT('Ctrl Pts',(-0.127808847501381,0.152298500092595,
-0.28486299302772));
#25543=CARTESIAN_POINT('Ctrl Pts',(-0.197529946699595,-0.0226241412066662,
-0.273870942420553));
#25544=CARTESIAN_POINT('Ctrl Pts',(-0.090063652484807,-0.177252553236508,
-0.262878891813384));
#25545=CARTESIAN_POINT('Ctrl Pts',(0.0981911158486954,-0.172882724045174,
-0.251886841206217));
#25546=CARTESIAN_POINT('Ctrl Pts',(0.198366949206078,-0.0134344343002136,
-0.240894790599049));
#25547=CARTESIAN_POINT('Ctrl Pts',(0.120604590887382,0.158064743757679,
-0.229902739991882));
#25548=CARTESIAN_POINT('Ctrl Pts',(-0.0653419364433495,0.18777742901298,
-0.218910689384714));
#25549=CARTESIAN_POINT('Ctrl Pts',(-0.192675739185548,0.0490508782497135,
-0.207918638777546));
#25550=CARTESIAN_POINT('Ctrl Pts',(-0.147176464299083,-0.133675053637187,
-0.196926588170379));
#25551=CARTESIAN_POINT('Ctrl Pts',(0.0303423782099813,-0.196492429153511,
-0.185934537563211));
#25552=CARTESIAN_POINT('Ctrl Pts',(0.180643596417653,-0.0830530570867919,
-0.174942486956044));
#25553=CARTESIAN_POINT('Ctrl Pts',(0.168904828983355,0.10488612646095,-0.163950436348876));
#25554=CARTESIAN_POINT('Ctrl Pts',(0.00565567373923916,0.198740949071929,
-0.152958385741709));
#25555=CARTESIAN_POINT('Ctrl Pts',(-0.16266638623247,0.114321901487825,
-0.14196633513454));
#25556=CARTESIAN_POINT('Ctrl Pts',(-0.185074818748011,-0.0726452733992181,
-0.130974284527373));
#25557=CARTESIAN_POINT('Ctrl Pts',(-0.0414671322339938,-0.194449231244725,
-0.119982233920205));
#25558=CARTESIAN_POINT('Ctrl Pts',(0.13933497184182,-0.141827901046976,
-0.108990183313038));
#25559=CARTESIAN_POINT('Ctrl Pts',(0.195155738897669,0.038012655435143,
-0.0979981327058701));
#25560=CARTESIAN_POINT('Ctrl Pts',(0.0759106707787678,0.183760191625162,
-0.0870060820987027));
#25561=CARTESIAN_POINT('Ctrl Pts',(-0.111411878022866,0.164662638746789,
-0.0760140314915348));
#25562=CARTESIAN_POINT('Ctrl Pts',(-0.198825961961294,-0.00212191126731689,
-0.0650219808843673));
#25563=CARTESIAN_POINT('Ctrl Pts',(-0.107833394863656,-0.167037292381857,
-0.0540299302771995));
#25564=CARTESIAN_POINT('Ctrl Pts',(0.0797788990713359,-0.1820521525943,
-0.043037879670032));
#25565=CARTESIAN_POINT('Ctrl Pts',(0.196037189143439,-0.0338901392339913,
-0.0320458290628643));
#25566=CARTESIAN_POINT('Ctrl Pts',(0.136032546505688,0.144928022941225,
-0.0210537784556966));
#25567=CARTESIAN_POINT('Ctrl Pts',(0.0152987425844774,0.177070029086086,
-0.0137257447175849));
#25568=CARTESIAN_POINT('Ctrl Pts',(-0.038745469013963,0.164327365570475,
-0.010061727848529));
#25569=CARTESIAN_POINT('Ctrl Pts',(0.0903606778650195,-0.126612599672284,
-0.453066666666667));
#25570=CARTESIAN_POINT('Ctrl Pts',(0.13200120501619,-0.0968946547775781,
-0.449402649797611));
#25571=CARTESIAN_POINT('Ctrl Pts',(0.183022071105112,0.00628961186891934,
-0.442074616059498));
#25572=CARTESIAN_POINT('Ctrl Pts',(0.0955251259476364,0.156432482487892,
-0.431082565452332));
#25573=CARTESIAN_POINT('Ctrl Pts',(-0.0777334665521386,0.165810192362521,
-0.420090514845164));
#25574=CARTESIAN_POINT('Ctrl Pts',(-0.18122493706769,0.0266753013132598,
-0.409098464237996));
#25575=CARTESIAN_POINT('Ctrl Pts',(-0.122175319415237,-0.136502693711184,
-0.398106413630829));
#25576=CARTESIAN_POINT('Ctrl Pts',(0.0464781498992043,-0.177175601660564,
-0.38711436302366));
#25577=CARTESIAN_POINT('Ctrl Pts',(0.17343439203133,-0.0589507354003139,
-0.376122312416494));
#25578=CARTESIAN_POINT('Ctrl Pts',(0.144820268191827,0.112170318563691,
-0.365130261809325));
#25579=CARTESIAN_POINT('Ctrl Pts',(-0.0137013956641988,0.182664248636804,
-0.354138211202158));
#25580=CARTESIAN_POINT('Ctrl Pts',(-0.159931890730855,0.0893100691219848,
-0.34314616059499));
#25581=CARTESIAN_POINT('Ctrl Pts',(-0.162701452047721,-0.0841589785101726,
-0.332154109987823));
#25582=CARTESIAN_POINT('Ctrl Pts',(-0.0195250965894654,-0.182134892710474,
-0.321162059380655));
#25583=CARTESIAN_POINT('Ctrl Pts',(0.141165453703306,-0.116733667162349,
-0.310170008773487));
#25584=CARTESIAN_POINT('Ctrl Pts',(0.175228489841733,0.0533797867075198,
-0.29917795816632));
#25585=CARTESIAN_POINT('Ctrl Pts',(0.052108853983618,0.175610575755033,
-0.288185907559152));
#25586=CARTESIAN_POINT('Ctrl Pts',(-0.117753205698952,0.140316081082348,
-0.277193856951985));
#25587=CARTESIAN_POINT('Ctrl Pts',(-0.181988844279104,-0.0208441372045229,
-0.266201806344817));
#25588=CARTESIAN_POINT('Ctrl Pts',(-0.0829776968055973,-0.163306819284929,
-0.255209755737649));
#25589=CARTESIAN_POINT('Ctrl Pts',(0.0904657141377962,-0.159280796003317,
-0.244217705130481));
#25590=CARTESIAN_POINT('Ctrl Pts',(0.182759993774958,-0.0123774506736319,
-0.233225654523314));
#25591=CARTESIAN_POINT('Ctrl Pts',(0.111115759797821,0.145628652861839,
-0.222233603916146));
#25592=CARTESIAN_POINT('Ctrl Pts',(-0.0602010160736213,0.173003627342364,
-0.211241553308979));
#25593=CARTESIAN_POINT('Ctrl Pts',(-0.17751655220323,0.045191692665802,
-0.200249502701811));
#25594=CARTESIAN_POINT('Ctrl Pts',(-0.135597032705167,-0.123157875182218,
-0.189257452094644));
#25595=CARTESIAN_POINT('Ctrl Pts',(0.0279551249589101,-0.181032955704809,
-0.178265401487475));
#25596=CARTESIAN_POINT('Ctrl Pts',(0.166431064695553,-0.0765186753989169,
-0.167273350880308));
#25597=CARTESIAN_POINT('Ctrl Pts',(0.15561587057272,0.0966339800849018,
-0.15628130027314));
#25598=CARTESIAN_POINT('Ctrl Pts',(0.00521070118542118,0.183104568379892,
-0.145289249665973));
#25599=CARTESIAN_POINT('Ctrl Pts',(-0.149868251007665,0.105327374786364,
-0.134297199058805));
#25600=CARTESIAN_POINT('Ctrl Pts',(-0.170513650876129,-0.0669297469531004,
-0.123305148451637));
#25601=CARTESIAN_POINT('Ctrl Pts',(-0.038204614525159,-0.179150510879271,
-0.11231309784447));
#25602=CARTESIAN_POINT('Ctrl Pts',(0.128372486890396,-0.130669279414751,
-0.101321047237302));
#25603=CARTESIAN_POINT('Ctrl Pts',(0.179801432490814,0.0350219262760309,
-0.0903289966301345));
#25604=CARTESIAN_POINT('Ctrl Pts',(0.0699382320215437,0.169302454929678,
-0.0793369460229671));
#25605=CARTESIAN_POINT('Ctrl Pts',(-0.102646303809221,0.151707443970759,
-0.0683448954157993));
#25606=CARTESIAN_POINT('Ctrl Pts',(-0.18318289269346,-0.00195496523769697,
-0.0573528448086317));
#25607=CARTESIAN_POINT('Ctrl Pts',(-0.0993493656725074,-0.153895266515289,
-0.0463607942014641));
#25608=CARTESIAN_POINT('Ctrl Pts',(0.0735021189568392,-0.167728799621184,
-0.0353687435942965));
#25609=CARTESIAN_POINT('Ctrl Pts',(0.18061353270244,-0.0312237580918893,
-0.0243766929871287));
#25610=CARTESIAN_POINT('Ctrl Pts',(0.125329887121183,0.133525492409719,
-0.0133846423799611));
#25611=CARTESIAN_POINT('Ctrl Pts',(0.0140950804087784,0.163138655622946,
-0.00605660864184936));
#25612=CARTESIAN_POINT('Ctrl Pts',(-0.0356970841369515,0.151398549148,-0.0023925917727935));
#25613=CARTESIAN_POINT('Ctrl Pts',(-0.044842238767986,0.190184998415424,
-0.0254000000000001));
#25614=CARTESIAN_POINT('Ctrl Pts',(0.0177060669358758,0.204932776012367,
-0.029064016869056));
#25615=CARTESIAN_POINT('Ctrl Pts',(0.0875719661052875,0.186332930008301,
-0.0327280337381119));
#25616=CARTESIAN_POINT('Ctrl Pts',(0.13407935514845,0.14254034275253,-0.0363920506071677));
#25617=CARTESIAN_POINT('Ctrl Pts',(0.180586744191612,0.0987477554967585,
-0.0400560674762236));
#25618=CARTESIAN_POINT('Ctrl Pts',(0.203735623108525,0.0297624269892805,
-0.0437200843452796));
#25619=CARTESIAN_POINT('Ctrl Pts',(0.192884722112796,-0.0333095634348471,
-0.0473841012143354));
#25620=CARTESIAN_POINT('Ctrl Pts',(0.182033821117068,-0.0963815538589742,
-0.0510481180833913));
#25621=CARTESIAN_POINT('Ctrl Pts',(0.137183140208699,-0.153540206199751,
-0.0547121349524471));
#25622=CARTESIAN_POINT('Ctrl Pts',(0.0785688143301349,-0.179223279965884,
-0.0583761518215029));
#25623=CARTESIAN_POINT('Ctrl Pts',(0.0199544884515696,-0.204906353732018,
-0.0620401686905588));
#25624=CARTESIAN_POINT('Ctrl Pts',(-0.0524234823971925,-0.199113848923506,
-0.0657041855596148));
#25625=CARTESIAN_POINT('Ctrl Pts',(-0.106164242363408,-0.16440667305451,
-0.0693682024286707));
#25626=CARTESIAN_POINT('Ctrl Pts',(-0.159905002329622,-0.129699497185515,
-0.0730322192977266));
#25627=CARTESIAN_POINT('Ctrl Pts',(-0.195008551413291,-0.0660776502560358,
-0.0766962361667824));
#25628=CARTESIAN_POINT('Ctrl Pts',(-0.195698813613992,-0.00209525485372862,
-0.0803602530358383));
#25629=CARTESIAN_POINT('Ctrl Pts',(-0.195706314304269,-0.00139999422583294,
-0.0804000678419734));
#25630=CARTESIAN_POINT('Ctrl Pts',(-0.195709751492929,-0.000704691024575797,
-0.0804398826481084));
#25631=CARTESIAN_POINT('Ctrl Pts',(-0.195709144608334,-9.38226522190222E-6,
-0.0804796974542435));
#25632=CARTESIAN_POINT('Origin',(0.,0.,-0.199));
#25633=CARTESIAN_POINT('',(0.0577350269189626,-0.1,-0.199));
#25634=CARTESIAN_POINT('',(-0.0577350269189627,-0.1,-0.199));
#25635=CARTESIAN_POINT('',(0.0288675134594813,-0.1,-0.199));
#25636=CARTESIAN_POINT('Origin',(0.,0.,-0.199));
#25637=CARTESIAN_POINT('Origin',(0.,0.,-0.199));
#25638=CARTESIAN_POINT('',(-0.115470053837925,2.77555756156289E-17,-0.199));
#25639=CARTESIAN_POINT('',(-0.0721687836487033,-0.075,-0.199));
#25640=CARTESIAN_POINT('Origin',(0.,0.,-0.199));
#25641=CARTESIAN_POINT('Origin',(0.,0.,-0.199));
#25642=CARTESIAN_POINT('',(-0.0577350269189626,0.1,-0.199));
#25643=CARTESIAN_POINT('',(-0.101036297108185,0.025,-0.199));
#25644=CARTESIAN_POINT('Origin',(0.,0.,-0.199));
#25645=CARTESIAN_POINT('Origin',(0.,0.,-0.199));
#25646=CARTESIAN_POINT('',(0.0577350269189626,0.1,-0.199));
#25647=CARTESIAN_POINT('',(-0.0288675134594813,0.1,-0.199));
#25648=CARTESIAN_POINT('Origin',(0.,0.,-0.199));
#25649=CARTESIAN_POINT('Origin',(0.,0.,-0.199));
#25650=CARTESIAN_POINT('',(0.115470053837925,0.,-0.199));
#25651=CARTESIAN_POINT('',(0.0721687836487032,0.075,-0.199));
#25652=CARTESIAN_POINT('Origin',(0.,0.,-0.199));
#25653=CARTESIAN_POINT('Origin',(0.,0.,-0.199));
#25654=CARTESIAN_POINT('',(0.101036297108185,-0.025,-0.199));
#25655=CARTESIAN_POINT('Origin',(0.,0.,-0.199));
#25656=CARTESIAN_POINT('Origin',(0.,0.,-0.234141016151378));
#25657=CARTESIAN_POINT('',(0.,0.,-0.269282032302755));
#25658=CARTESIAN_POINT('',(-0.113827101150665,-1.39397995080384E-17,-0.2));
#25659=CARTESIAN_POINT('',(-0.0577350269189626,-7.07050159149938E-18,-0.234141016151378));
#25660=CARTESIAN_POINT('',(-0.113789894775128,-0.00291012086156119,-0.2));
#25661=CARTESIAN_POINT('Origin',(0.,0.,-0.2));
#25662=CARTESIAN_POINT('Ctrl Pts',(-0.115470053837925,-1.38777878078145E-17,
-0.199));
#25663=CARTESIAN_POINT('Ctrl Pts',(-0.114623954995367,-0.00146548618353618,
-0.199514986736453));
#25664=CARTESIAN_POINT('Ctrl Pts',(-0.113789894775128,-0.00291012086156124,
-0.2));
#25665=CARTESIAN_POINT('',(-0.0594151859817593,-0.0970898791384388,-0.2));
#25666=CARTESIAN_POINT('Ctrl Pts',(-0.0594151859817594,-0.0970898791384387,
-0.2));
#25667=CARTESIAN_POINT('Ctrl Pts',(-0.0585811257615208,-0.0985345138164641,
-0.199514986736453));
#25668=CARTESIAN_POINT('Ctrl Pts',(-0.0577350269189627,-0.1,-0.199));
#25669=CARTESIAN_POINT('',(-0.0543747087933692,-0.1,-0.2));
#25670=CARTESIAN_POINT('Origin',(0.,0.,-0.2));
#25671=CARTESIAN_POINT('Ctrl Pts',(-0.0577350269189627,-0.1,-0.199));
#25672=CARTESIAN_POINT('Ctrl Pts',(-0.0560428292338519,-0.1,-0.199514986736451));
#25673=CARTESIAN_POINT('Ctrl Pts',(-0.0543747087933692,-0.1,-0.2));
#25674=CARTESIAN_POINT('',(0.0543747087933691,-0.1,-0.2));
#25675=CARTESIAN_POINT('Ctrl Pts',(0.0543747087933691,-0.1,-0.2));
#25676=CARTESIAN_POINT('Ctrl Pts',(0.056042829233854,-0.1,-0.19951498673645));
#25677=CARTESIAN_POINT('Ctrl Pts',(0.0577350269189626,-0.1,-0.199));
#25678=CARTESIAN_POINT('',(0.0594151859817594,-0.0970898791384387,-0.2));
#25679=CARTESIAN_POINT('Origin',(0.,0.,-0.2));
#25680=CARTESIAN_POINT('Ctrl Pts',(0.0577350269189626,-0.1,-0.199));
#25681=CARTESIAN_POINT('Ctrl Pts',(0.0585811257615188,-0.0985345138164674,
-0.199514986736451));
#25682=CARTESIAN_POINT('Ctrl Pts',(0.0594151859817594,-0.0970898791384387,
-0.2));
#25683=CARTESIAN_POINT('',(0.113789894775128,-0.00291012086156127,-0.2));
#25684=CARTESIAN_POINT('Ctrl Pts',(0.113789894775128,-0.00291012086156127,
-0.2));
#25685=CARTESIAN_POINT('Ctrl Pts',(0.114623954995369,-0.00146548618353307,
-0.199514986736452));
#25686=CARTESIAN_POINT('Ctrl Pts',(0.115470053837925,1.38777878078145E-17,
-0.199));
#25687=CARTESIAN_POINT('',(0.113789894775128,0.00291012086156127,-0.2));
#25688=CARTESIAN_POINT('Origin',(0.,0.,-0.2));
#25689=CARTESIAN_POINT('Ctrl Pts',(0.115470053837925,0.,-0.199));
#25690=CARTESIAN_POINT('Ctrl Pts',(0.114623954995369,0.00146548618353293,
-0.199514986736452));
#25691=CARTESIAN_POINT('Ctrl Pts',(0.113789894775128,0.00291012086156128,
-0.2));
#25692=CARTESIAN_POINT('',(0.0594151859817593,0.0970898791384387,-0.2));
#25693=CARTESIAN_POINT('Ctrl Pts',(0.0594151859817593,0.0970898791384387,
-0.2));
#25694=CARTESIAN_POINT('Ctrl Pts',(0.0585811257615177,0.0985345138164694,
-0.199514986736451));
#25695=CARTESIAN_POINT('Ctrl Pts',(0.0577350269189626,0.1,-0.199));
#25696=CARTESIAN_POINT('',(0.0543747087933691,0.1,-0.2));
#25697=CARTESIAN_POINT('Origin',(0.,0.,-0.2));
#25698=CARTESIAN_POINT('Ctrl Pts',(0.0577350269189626,0.1,-0.199));
#25699=CARTESIAN_POINT('Ctrl Pts',(0.0560428292338471,0.1,-0.199514986736452));
#25700=CARTESIAN_POINT('Ctrl Pts',(0.0543747087933691,0.1,-0.2));
#25701=CARTESIAN_POINT('',(-0.0543747087933691,0.1,-0.2));
#25702=CARTESIAN_POINT('Ctrl Pts',(-0.0543747087933691,0.1,-0.2));
#25703=CARTESIAN_POINT('Ctrl Pts',(-0.0560428292338464,0.1,-0.199514986736453));
#25704=CARTESIAN_POINT('Ctrl Pts',(-0.0577350269189626,0.1,-0.199));
#25705=CARTESIAN_POINT('',(-0.0594151859817593,0.0970898791384387,-0.2));
#25706=CARTESIAN_POINT('Origin',(0.,0.,-0.2));
#25707=CARTESIAN_POINT('Ctrl Pts',(-0.0577350269189626,0.1,-0.199));
#25708=CARTESIAN_POINT('Ctrl Pts',(-0.0585811257615179,0.0985345138164689,
-0.199514986736451));
#25709=CARTESIAN_POINT('Ctrl Pts',(-0.0594151859817593,0.0970898791384388,
-0.2));
#25710=CARTESIAN_POINT('',(-0.113789894775128,0.0029101208615613,-0.2));
#25711=CARTESIAN_POINT('Ctrl Pts',(-0.113789894775128,0.00291012086156131,
-0.2));
#25712=CARTESIAN_POINT('Ctrl Pts',(-0.11462395499537,0.00146548618353128,
-0.199514986736451));
#25713=CARTESIAN_POINT('Ctrl Pts',(-0.115470053837925,2.08166817117217E-17,
-0.199));
#25714=CARTESIAN_POINT('Origin',(0.,0.,-0.2));
#25715=CARTESIAN_POINT('Origin',(-0.115470053837925,1.38777878078145E-17,
0.));
#25716=CARTESIAN_POINT('',(-0.0577350269189626,0.1,0.));
#25717=CARTESIAN_POINT('',(-0.0577350269189626,0.1,0.));
#25718=CARTESIAN_POINT('',(-0.115470053837925,1.41410031829988E-17,0.));
#25719=CARTESIAN_POINT('',(-0.101036297108185,0.025,0.));
#25720=CARTESIAN_POINT('',(-0.115470053837925,1.41410031829988E-17,0.));
#25721=CARTESIAN_POINT('Origin',(-0.115470053837925,1.38777878078145E-17,
0.));
#25722=CARTESIAN_POINT('',(-0.115470053837925,1.38777878078145E-17,-0.2));
#25723=CARTESIAN_POINT('',(-0.115470053837925,1.41410031829988E-17,0.));
#25724=CARTESIAN_POINT('',(-0.0577350269189626,0.1,-0.2));
#25725=CARTESIAN_POINT('Origin',(-0.0577350269189626,0.1,0.));
#25726=CARTESIAN_POINT('',(0.0577350269189626,0.1,0.));
#25727=CARTESIAN_POINT('',(0.0577350269189626,0.1,0.));
#25728=CARTESIAN_POINT('',(-0.0288675134594813,0.1,0.));
#25729=CARTESIAN_POINT('Origin',(-0.0577350269189626,0.1,0.));
#25730=CARTESIAN_POINT('',(0.0577350269189626,0.1,-0.2));
#25731=CARTESIAN_POINT('',(0.0577350269189626,0.1,-0.2));
#25732=CARTESIAN_POINT('',(0.0577350269189626,0.1,0.));
#25733=CARTESIAN_POINT('Origin',(-0.0577350269189626,0.1,0.));
#25734=CARTESIAN_POINT('',(-0.0577350269189626,0.1,-0.2));
#25735=CARTESIAN_POINT('',(-0.0577350269189626,0.1,0.));
#25736=CARTESIAN_POINT('',(0.0577350269189626,0.1,-0.2));
#25737=CARTESIAN_POINT('Origin',(-0.0577350269189626,-0.1,0.));
#25738=CARTESIAN_POINT('',(-0.0577350269189626,-0.1,0.));
#25739=CARTESIAN_POINT('',(-0.0721687836487033,-0.075,0.));
#25740=CARTESIAN_POINT('',(-0.0577350269189626,-0.1,0.));
#25741=CARTESIAN_POINT('Origin',(-0.0577350269189626,-0.1,0.));
#25742=CARTESIAN_POINT('',(-0.0577350269189626,-0.1,-0.2));
#25743=CARTESIAN_POINT('',(-0.0577350269189626,-0.1,0.));
#25744=CARTESIAN_POINT('',(-0.115470053837925,1.41410031829988E-17,-0.2));
#25745=CARTESIAN_POINT('Origin',(0.0577350269189626,0.1,0.));
#25746=CARTESIAN_POINT('',(0.115470053837925,0.,0.));
#25747=CARTESIAN_POINT('',(0.115470053837925,0.,0.));
#25748=CARTESIAN_POINT('',(0.0721687836487032,0.075,0.));
#25749=CARTESIAN_POINT('Origin',(0.0577350269189626,0.1,0.));
#25750=CARTESIAN_POINT('',(0.115470053837925,0.,-0.2));
#25751=CARTESIAN_POINT('',(0.115470053837925,0.,-0.2));
#25752=CARTESIAN_POINT('',(0.115470053837925,0.,0.));
#25753=CARTESIAN_POINT('Origin',(0.0577350269189626,0.1,0.));
#25754=CARTESIAN_POINT('',(0.115470053837925,0.,-0.2));
#25755=CARTESIAN_POINT('Origin',(0.,0.,-0.2));
#25756=CARTESIAN_POINT('',(-0.0577350269189626,0.1,-0.2));
#25757=CARTESIAN_POINT('Origin',(0.,0.,-0.2));
#25758=CARTESIAN_POINT('Origin',(0.,0.,-0.2));
#25759=CARTESIAN_POINT('',(0.0577350269189626,-0.1,-0.2));
#25760=CARTESIAN_POINT('Origin',(0.,0.,-0.2));
#25761=CARTESIAN_POINT('',(0.0577350269189626,-0.1,-0.2));
#25762=CARTESIAN_POINT('',(-0.0577350269189626,-0.1,-0.2));
#25763=CARTESIAN_POINT('',(0.0577350269189626,-0.1,-0.2));
#25764=CARTESIAN_POINT('Origin',(0.,0.,-0.2));
#25765=CARTESIAN_POINT('',(-0.0577350269189626,-0.1,-0.2));
#25766=CARTESIAN_POINT('Origin',(0.,0.,-0.2));
#25767=CARTESIAN_POINT('',(-0.115470053837925,1.41410031829988E-17,-0.2));
#25768=CARTESIAN_POINT('Origin',(0.115470053837925,0.,0.));
#25769=CARTESIAN_POINT('',(0.0577350269189626,-0.1,0.));
#25770=CARTESIAN_POINT('',(0.0577350269189626,-0.1,0.));
#25771=CARTESIAN_POINT('',(0.101036297108185,-0.025,0.));
#25772=CARTESIAN_POINT('Origin',(0.115470053837925,0.,0.));
#25773=CARTESIAN_POINT('',(0.0577350269189626,-0.1,0.));
#25774=CARTESIAN_POINT('Origin',(0.115470053837925,0.,0.));
#25775=CARTESIAN_POINT('Origin',(0.0577350269189626,-0.1,0.));
#25776=CARTESIAN_POINT('Origin',(0.0577350269189626,-0.1,0.));
#25777=CARTESIAN_POINT('',(0.0288675134594813,-0.1,0.));
#25778=CARTESIAN_POINT('Origin',(-0.115470053837925,1.38777878078145E-17,
0.));
#25779=CARTESIAN_POINT('Origin',(-0.0577350269189626,-0.1,0.));
#25780=CARTESIAN_POINT('Origin',(0.0577350269189626,-0.1,0.));
#25781=CARTESIAN_POINT('Origin',(0.125,0.,-0.5));
#25782=CARTESIAN_POINT('',(-0.125,-1.53080849893419E-17,-0.5));
#25783=CARTESIAN_POINT('Origin',(0.,0.,-0.5));
#25784=CARTESIAN_POINT('Origin',(0.,0.,-0.475));
#25785=CARTESIAN_POINT('',(-0.1625,-1.99005104861445E-17,-0.475));
#25786=CARTESIAN_POINT('Origin',(0.,0.,-0.24));
#25787=CARTESIAN_POINT('Origin',(0.,0.,-0.0254000000000001));
#25788=CARTESIAN_POINT('Origin',(0.,0.,-0.015));
#25789=CARTESIAN_POINT('',(-0.17,-2.0818995585505E-17,-1.73472347597681E-18));
#25790=CARTESIAN_POINT('Origin',(0.,0.,0.));
#25791=CARTESIAN_POINT('',(-0.185,-2.2655965784226E-17,-0.015));
#25792=CARTESIAN_POINT('Origin',(0.,0.,0.));
#25793=CARTESIAN_POINT('',(0.,0.,0.));
#25794=CARTESIAN_POINT('Origin',(0.,0.,-0.19));
#25795=CARTESIAN_POINT('',(-0.195529498469593,0.00015768127982491,-0.330479697454243));
#25796=CARTESIAN_POINT('',(-0.195550405894074,0.000204984114986345,-0.34065363587909));
#25797=CARTESIAN_POINT('',(-0.1954,-2.39295984553393E-17,-0.19));
#25798=CARTESIAN_POINT('',(0.0862527678113333,0.175483407289205,-0.353066666666667));
#25799=CARTESIAN_POINT('Ctrl Pts',(-0.195529498469593,0.00015768127982491,
-0.330479697454243));
#25800=CARTESIAN_POINT('Ctrl Pts',(-0.195614985209273,0.0104270003956845,
-0.331066403480209));
#25801=CARTESIAN_POINT('Ctrl Pts',(-0.194873746209122,0.0206833915158047,
-0.331653109506174));
#25802=CARTESIAN_POINT('Ctrl Pts',(-0.193261993352752,0.0308003123059383,
-0.332239815532139));
#25803=CARTESIAN_POINT('Ctrl Pts',(-0.183227156255684,0.0937886616993844,
-0.33589267047895));
#25804=CARTESIAN_POINT('Ctrl Pts',(-0.139448095221308,0.151370643331935,
-0.339545525425761));
#25805=CARTESIAN_POINT('Ctrl Pts',(-0.0814380303326093,0.177933707035516,
-0.343198380372573));
#25806=CARTESIAN_POINT('Ctrl Pts',(-0.0291994446604737,0.201853985036518,
-0.346487809137271));
#25807=CARTESIAN_POINT('Ctrl Pts',(0.034579296332332,0.200620511802275,
-0.349777237901969));
#25808=CARTESIAN_POINT('Ctrl Pts',(0.0863529496556118,0.175584683415657,
-0.353066666666667));
#25809=CARTESIAN_POINT('',(-0.0861525859670515,0.175382131162755,-0.353066666666667));
#25810=CARTESIAN_POINT('Origin',(0.,0.,-0.353066666666667));
#25811=CARTESIAN_POINT('Ctrl Pts',(-0.0861525859670515,0.175382131162755,
-0.353066666666667));
#25812=CARTESIAN_POINT('Ctrl Pts',(-0.143656790266726,0.147134464929317,
-0.349413811719856));
#25813=CARTESIAN_POINT('Ctrl Pts',(-0.185739203174332,0.0886770108875964,
-0.345760956773044));
#25814=CARTESIAN_POINT('Ctrl Pts',(-0.194015268225219,0.0255264096968064,
-0.342108101826233));
#25815=CARTESIAN_POINT('Ctrl Pts',(-0.195113701730712,0.0171448013100274,
-0.341623279843852));
#25816=CARTESIAN_POINT('Ctrl Pts',(-0.195616612964559,0.00868051988020842,
-0.341138457861471));
#25817=CARTESIAN_POINT('Ctrl Pts',(-0.195550405894074,0.000204984114986345,
-0.34065363587909));
#25818=CARTESIAN_POINT('Origin',(0.,0.,-0.19));
#25819=CARTESIAN_POINT('',(-0.195110707760101,-4.72585694041849E-5,-0.260479697454244));
#25820=CARTESIAN_POINT('',(-0.195100849729129,-1.92665112341343E-5,-0.27065363587909));
#25821=CARTESIAN_POINT('',(-0.1954,-2.39295984553393E-17,-0.19));
#25822=CARTESIAN_POINT('Ctrl Pts',(-0.195110707760101,-4.72585694041849E-5,
-0.260479697454244));
#25823=CARTESIAN_POINT('Ctrl Pts',(-0.19503202637266,0.0352043980738878,
-0.262482607132675));
#25824=CARTESIAN_POINT('Ctrl Pts',(-0.185884422793289,0.0704940830525105,
-0.264485516811107));
#25825=CARTESIAN_POINT('Ctrl Pts',(-0.167920692172535,0.100506798190785,
-0.266488426489538));
#25826=CARTESIAN_POINT('Ctrl Pts',(-0.135158904175888,0.155243212988051,
-0.270141281436349));
#25827=CARTESIAN_POINT('Ctrl Pts',(-0.073073335453198,0.192427622718924,
-0.27379413638316));
#25828=CARTESIAN_POINT('Ctrl Pts',(-0.00935407487596699,0.195477079378747,
-0.277446991329971));
#25829=CARTESIAN_POINT('Ctrl Pts',(0.0543651857012641,0.19852653603857,
-0.281099846276782));
#25830=CARTESIAN_POINT('Ctrl Pts',(0.119718138133036,0.167441039627343,
-0.284752701223594));
#25831=CARTESIAN_POINT('Ctrl Pts',(0.157556692003627,0.116082124071139,
-0.288405556170405));
#25832=CARTESIAN_POINT('Ctrl Pts',(0.195395245874219,0.0647232085149348,
-0.292058411117216));
#25833=CARTESIAN_POINT('Ctrl Pts',(0.205719401183631,-0.00690912618624702,
-0.295711266064027));
#25834=CARTESIAN_POINT('Ctrl Pts',(0.183925482710756,-0.0668615165007966,
-0.299364121010839));
#25835=CARTESIAN_POINT('Ctrl Pts',(0.16213156423788,-0.126813906815346,
-0.30301697595765));
#25836=CARTESIAN_POINT('Ctrl Pts',(0.108219571982719,-0.175086352743264,
-0.306669830904461));
#25837=CARTESIAN_POINT('Ctrl Pts',(0.0462326364389881,-0.19015902116139,
-0.310322685851272));
#25838=CARTESIAN_POINT('Ctrl Pts',(-0.0157542991047424,-0.205231689579517,
-0.313975540798083));
#25839=CARTESIAN_POINT('Ctrl Pts',(-0.0858161779370413,-0.187104580487853,
-0.317628395744894));
#25840=CARTESIAN_POINT('Ctrl Pts',(-0.132701810773311,-0.143843667364851,
-0.321281250691706));
#25841=CARTESIAN_POINT('Ctrl Pts',(-0.172056872668009,-0.107531138119007,
-0.324347399612552));
#25842=CARTESIAN_POINT('Ctrl Pts',(-0.195082741383395,-0.0535101870075604,
-0.327413548533398));
#25843=CARTESIAN_POINT('Ctrl Pts',(-0.195529498469593,0.00015768127982491,
-0.330479697454243));
#25844=CARTESIAN_POINT('Ctrl Pts',(-0.195550405894074,0.000204984114986345,
-0.34065363587909));
#25845=CARTESIAN_POINT('Ctrl Pts',(-0.195117780746291,-0.0551777701148348,
-0.33748560291466));
#25846=CARTESIAN_POINT('Ctrl Pts',(-0.170384536859063,-0.111041069974121,
-0.33431756995023));
#25847=CARTESIAN_POINT('Ctrl Pts',(-0.128717685823896,-0.147458271836019,
-0.3311495369858));
#25848=CARTESIAN_POINT('Ctrl Pts',(-0.0806743211775187,-0.189448603838194,
-0.327496682038988));
#25849=CARTESIAN_POINT('Ctrl Pts',(-0.0101178746905964,-0.205585519502686,
-0.323843827092177));
#25850=CARTESIAN_POINT('Ctrl Pts',(0.0514379301081016,-0.188803240428617,
-0.320190972145366));
#25851=CARTESIAN_POINT('Ctrl Pts',(0.1129937349068,-0.172020961354547,-0.316538117198555));
#25852=CARTESIAN_POINT('Ctrl Pts',(0.165548898017274,-0.122319487541918,
-0.312885262251744));
#25853=CARTESIAN_POINT('Ctrl Pts',(0.18568706648142,-0.0617993993866737,
-0.309232407304933));
#25854=CARTESIAN_POINT('Ctrl Pts',(0.205825234945567,-0.00127931123142962,
-0.305579552358121));
#25855=CARTESIAN_POINT('Ctrl Pts',(0.193546408763386,0.0700593912664289,
-0.30192669741131));
#25856=CARTESIAN_POINT('Ctrl Pts',(0.154314767542849,0.120364936306517,
-0.298273842464499));
#25857=CARTESIAN_POINT('Ctrl Pts',(0.115083126322312,0.170670481346605,
-0.294620987517688));
#25858=CARTESIAN_POINT('Ctrl Pts',(0.0488986700634175,0.199942868928924,
-0.290968132570877));
#25859=CARTESIAN_POINT('Ctrl Pts',(-0.0147137545984364,0.195144562135855,
-0.287315277624065));
#25860=CARTESIAN_POINT('Ctrl Pts',(-0.0783261792602905,0.190346255342787,
-0.283662422677254));
#25861=CARTESIAN_POINT('Ctrl Pts',(-0.139366572325104,0.151477254174331,
-0.280009567730443));
#25862=CARTESIAN_POINT('Ctrl Pts',(-0.170614086184577,0.0958638092691071,
-0.276356712783632));
#25863=CARTESIAN_POINT('Ctrl Pts',(-0.186875976058951,0.0669213557782296,
-0.274455687148784));
#25864=CARTESIAN_POINT('Ctrl Pts',(-0.195068794346351,0.0334438550277428,
-0.272554661513937));
#25865=CARTESIAN_POINT('Ctrl Pts',(-0.195100849729129,-1.92665112341343E-5,
-0.27065363587909));
#25866=CARTESIAN_POINT('Origin',(0.,0.,-0.19));
#25867=CARTESIAN_POINT('',(-0.195668453670677,-6.92573205455238E-5,-0.190479697454244));
#25868=CARTESIAN_POINT('',(-0.195637235488324,-9.58052375767378E-5,-0.20065363587909));
#25869=CARTESIAN_POINT('',(-0.1954,-2.39295984553393E-17,-0.19));
#25870=CARTESIAN_POINT('Ctrl Pts',(-0.195668453670677,-6.92573205455238E-5,
-0.190479697454244));
#25871=CARTESIAN_POINT('Ctrl Pts',(-0.195389991269708,0.0596676372169134,
-0.193898810785141));
#25872=CARTESIAN_POINT('Ctrl Pts',(-0.165981871671571,0.119642236981856,
-0.197317924116039));
#25873=CARTESIAN_POINT('Ctrl Pts',(-0.118451210421177,0.155782728391626,
-0.200737037446937));
#25874=CARTESIAN_POINT('Ctrl Pts',(-0.0676711998538972,0.194393900368106,
-0.204389892393748));
#25875=CARTESIAN_POINT('Ctrl Pts',(0.00379387942481049,0.205800821502601,
-0.208042747340559));
#25876=CARTESIAN_POINT('Ctrl Pts',(0.0640703860629371,0.18491600234246,
-0.21169560228737));
#25877=CARTESIAN_POINT('Ctrl Pts',(0.124346892701064,0.164031183182318,
-0.215348457234181));
#25878=CARTESIAN_POINT('Ctrl Pts',(0.17343482669861,0.110854623727541,-0.219001312180993));
#25879=CARTESIAN_POINT('Ctrl Pts',(0.189440826068912,0.0491031668771414,
-0.222654167127804));
#25880=CARTESIAN_POINT('Ctrl Pts',(0.205446825439215,-0.0126482899732578,
-0.226307022074615));
#25881=CARTESIAN_POINT('Ctrl Pts',(0.188370890182274,-0.0829746442192793,
-0.229959877021426));
#25882=CARTESIAN_POINT('Ctrl Pts',(0.145828951483188,-0.130510033480858,
-0.233612731968237));
#25883=CARTESIAN_POINT('Ctrl Pts',(0.103287012784103,-0.178045422742437,
-0.237265586915048));
#25884=CARTESIAN_POINT('Ctrl Pts',(0.0352790706428725,-0.202789847019573,
-0.24091844186186));
#25885=CARTESIAN_POINT('Ctrl Pts',(-0.0278631709630815,-0.193707423330989,
-0.244571296808671));
#25886=CARTESIAN_POINT('Ctrl Pts',(-0.091005412569035,-0.184624999642405,
-0.248224151755482));
#25887=CARTESIAN_POINT('Ctrl Pts',(-0.149281953639712,-0.141715727988102,
-0.251877006702293));
#25888=CARTESIAN_POINT('Ctrl Pts',(-0.176701220539749,-0.0841168822291211,
-0.255529861649104));
#25889=CARTESIAN_POINT('Ctrl Pts',(-0.18908613325676,-0.0581002611456236,
-0.257179806917484));
#25890=CARTESIAN_POINT('Ctrl Pts',(-0.195175523455146,-0.02908666294569,
-0.258829752185864));
#25891=CARTESIAN_POINT('Ctrl Pts',(-0.195110707760101,-4.72585694041849E-5,
-0.260479697454244));
#25892=CARTESIAN_POINT('Ctrl Pts',(-0.195100849729129,-1.92665112341343E-5,
-0.27065363587909));
#25893=CARTESIAN_POINT('Ctrl Pts',(-0.195130389340867,-0.0308561348349446,
-0.268901806567126));
#25894=CARTESIAN_POINT('Ctrl Pts',(-0.188229846664525,-0.0616807923984399,
-0.267149977255162));
#25895=CARTESIAN_POINT('Ctrl Pts',(-0.174327468766743,-0.0889330908388636,
-0.265398147943198));
#25896=CARTESIAN_POINT('Ctrl Pts',(-0.145338702835303,-0.145758657399616,
-0.261745292996387));
#25897=CARTESIAN_POINT('Ctrl Pts',(-0.0859065363182925,-0.187051901879128,
-0.258092438049576));
#25898=CARTESIAN_POINT('Ctrl Pts',(-0.022538802750656,-0.194398503605164,
-0.254439583102765));
#25899=CARTESIAN_POINT('Ctrl Pts',(0.0408289308169802,-0.201745105331199,
-0.250786728155954));
#25900=CARTESIAN_POINT('Ctrl Pts',(0.108132231435242,-0.175145064303758,
-0.247133873209142));
#25901=CARTESIAN_POINT('Ctrl Pts',(0.149354112356093,-0.126460722080181,
-0.243481018262331));
#25902=CARTESIAN_POINT('Ctrl Pts',(0.190575993276944,-0.077776379856603,
-0.23982816331552));
#25903=CARTESIAN_POINT('Ctrl Pts',(0.205716454500384,-0.00700773643688812,
-0.236175308368709));
#25904=CARTESIAN_POINT('Ctrl Pts',(0.188022556237584,0.0542814807221939,
-0.232522453421898));
#25905=CARTESIAN_POINT('Ctrl Pts',(0.170328657974784,0.115570697881275,
-0.228869598475086));
#25906=CARTESIAN_POINT('Ctrl Pts',(0.119800400225746,0.167380488779724,
-0.225216743528275));
#25907=CARTESIAN_POINT('Ctrl Pts',(0.0589736618385814,0.186603908499629,
-0.221563888581464));
#25908=CARTESIAN_POINT('Ctrl Pts',(-0.00185307654858394,0.205827328219534,
-0.217911033634653));
#25909=CARTESIAN_POINT('Ctrl Pts',(-0.072978295573876,0.192464376760895,
-0.214258178687842));
#25910=CARTESIAN_POINT('Ctrl Pts',(-0.122680009238483,0.152474774305509,
-0.21060532374103));
#25911=CARTESIAN_POINT('Ctrl Pts',(-0.167815111124156,0.116159431269827,
-0.207288094453717));
#25912=CARTESIAN_POINT('Ctrl Pts',(-0.195282649515434,0.0578855880163676,
-0.203970865166403));
#25913=CARTESIAN_POINT('Ctrl Pts',(-0.195637235488324,-9.58052375767378E-5,
-0.20065363587909));
#25914=CARTESIAN_POINT('Origin',(0.,0.,-0.19));
#25915=CARTESIAN_POINT('',(-0.195243803960011,0.00014500399526908,-0.120479697454244));
#25916=CARTESIAN_POINT('',(-0.19528814483522,0.000156602802769957,-0.13065363587909));
#25917=CARTESIAN_POINT('',(-0.1954,-2.39295984553393E-17,-0.19));
#25918=CARTESIAN_POINT('Ctrl Pts',(-0.195243803960011,0.00014500399526908,
-0.120479697454244));
#25919=CARTESIAN_POINT('Ctrl Pts',(-0.195392189818952,0.0209208269505307,
-0.121662159490796));
#25920=CARTESIAN_POINT('Ctrl Pts',(-0.192328368303915,0.0416539845471214,
-0.122844621527349));
#25921=CARTESIAN_POINT('Ctrl Pts',(-0.185863548863049,0.0612660467409409,
-0.124027083563902));
#25922=CARTESIAN_POINT('Ctrl Pts',(-0.165892465695211,0.121851516876383,
-0.127679938510713));
#25923=CARTESIAN_POINT('Ctrl Pts',(-0.113465247009462,0.171738237669897,
-0.131332793457524));
#25924=CARTESIAN_POINT('Ctrl Pts',(-0.0519631608745109,0.18867645654452,
-0.134985648404335));
#25925=CARTESIAN_POINT('Ctrl Pts',(0.00953892526044009,0.205614675419143,
-0.138638503351147));
#25926=CARTESIAN_POINT('Ctrl Pts',(0.0801158788445938,0.189604392374876,
-0.142291358297958));
#25927=CARTESIAN_POINT('Ctrl Pts',(0.128289431003563,0.147786308936136,
-0.145944213244769));
#25928=CARTESIAN_POINT('Ctrl Pts',(0.176462983162532,0.105968225497396,
-0.14959706819158));
#25929=CARTESIAN_POINT('Ctrl Pts',(0.202233133896316,0.0383423416641833,
-0.153249923138391));
#25930=CARTESIAN_POINT('Ctrl Pts',(0.194106710935588,-0.0249300405017104,
-0.156902778085202));
#25931=CARTESIAN_POINT('Ctrl Pts',(0.18598028797486,-0.0882024226676044,
-0.160555633032014));
#25932=CARTESIAN_POINT('Ctrl Pts',(0.143957291319619,-0.147121303166179,
-0.164208487978825));
#25933=CARTESIAN_POINT('Ctrl Pts',(0.086779895216793,-0.175408670583934,
-0.167861342925636));
#25934=CARTESIAN_POINT('Ctrl Pts',(0.0296024991139669,-0.20369603800169,
-0.171514197872447));
#25935=CARTESIAN_POINT('Ctrl Pts',(-0.0427292964364452,-0.201351892338625,
-0.175167052819258));
#25936=CARTESIAN_POINT('Ctrl Pts',(-0.0979551963305346,-0.169421743264796,
-0.178819907766069));
#25937=CARTESIAN_POINT('Ctrl Pts',(-0.153181096224624,-0.137491594190968,
-0.182472762712881));
#25938=CARTESIAN_POINT('Ctrl Pts',(-0.191301100462392,-0.0759754417063763,
-0.186125617659692));
#25939=CARTESIAN_POINT('Ctrl Pts',(-0.19531363165335,-0.0123096540548478,
-0.189778472606503));
#25940=CARTESIAN_POINT('Ctrl Pts',(-0.195570388501934,-0.00823575999095568,
-0.190012214222417));
#25941=CARTESIAN_POINT('Ctrl Pts',(-0.195687490258609,-0.00415306411707918,
-0.19024595583833));
#25942=CARTESIAN_POINT('Ctrl Pts',(-0.195668453670677,-6.92573205455238E-5,
-0.190479697454244));
#25943=CARTESIAN_POINT('Ctrl Pts',(-0.195637235488324,-9.58052375767378E-5,
-0.20065363587909));
#25944=CARTESIAN_POINT('Ctrl Pts',(-0.195673111257133,-0.00596215985583099,
-0.200318010219592));
#25945=CARTESIAN_POINT('Ctrl Pts',(-0.195431440278219,-0.0118255207556224,
-0.199982384560095));
#25946=CARTESIAN_POINT('Ctrl Pts',(-0.194902439849197,-0.0176628423614353,
-0.199646758900597));
#25947=CARTESIAN_POINT('Ctrl Pts',(-0.189144948491384,-0.0811946031208615,
-0.195993903953786));
#25948=CARTESIAN_POINT('Ctrl Pts',(-0.149351757471835,-0.14164187118758,
-0.192341049006975));
#25949=CARTESIAN_POINT('Ctrl Pts',(-0.0932707556744568,-0.172045046060018,
-0.188688194060163));
#25950=CARTESIAN_POINT('Ctrl Pts',(-0.0371897538770789,-0.202448220932456,
-0.185035339113352));
#25951=CARTESIAN_POINT('Ctrl Pts',(0.0351790586981286,-0.202807302610614,
-0.181382484166541));
#25952=CARTESIAN_POINT('Ctrl Pts',(0.0915589780120191,-0.17296210786544,
-0.17772962921973));
#25953=CARTESIAN_POINT('Ctrl Pts',(0.14793889732591,-0.143116913120265,
-0.174076774272919));
#25954=CARTESIAN_POINT('Ctrl Pts',(0.188329923378484,-0.0830674419517585,
-0.170423919326108));
#25955=CARTESIAN_POINT('Ctrl Pts',(0.194717565566022,-0.0195959536108856,
-0.166771064379296));
#25956=CARTESIAN_POINT('Ctrl Pts',(0.20110520775356,0.043875534729987,-0.163118209432485));
#25957=CARTESIAN_POINT('Ctrl Pts',(0.173489466076062,0.110769040243225,
-0.159465354485674));
#25958=CARTESIAN_POINT('Ctrl Pts',(0.124186989019549,0.151249888653556,
-0.155812499538863));
#25959=CARTESIAN_POINT('Ctrl Pts',(0.0748845119630359,0.191730737063888,
-0.152159644592052));
#25960=CARTESIAN_POINT('Ctrl Pts',(0.00389529952750602,0.205798928371311,
-0.148506789645241));
#25961=CARTESIAN_POINT('Ctrl Pts',(-0.0571191521156268,0.187179977369007,
-0.144853934698429));
#25962=CARTESIAN_POINT('Ctrl Pts',(-0.118133603758759,0.168561026366703,
-0.141201079751618));
#25963=CARTESIAN_POINT('Ctrl Pts',(-0.169173294609495,0.117254933054672,
-0.137548224804807));
#25964=CARTESIAN_POINT('Ctrl Pts',(-0.187474573932762,0.0561444172355426,
-0.133895369857996));
#25965=CARTESIAN_POINT('Ctrl Pts',(-0.192888410498366,0.0380668643366071,
-0.132814791865027));
#25966=CARTESIAN_POINT('Ctrl Pts',(-0.195437376622097,0.0191313467738501,
-0.131734213872058));
#25967=CARTESIAN_POINT('Ctrl Pts',(-0.19528814483522,0.000156602802769957,
-0.13065363587909));
#25968=CARTESIAN_POINT('Origin',(0.,0.,-0.19));
#25969=CARTESIAN_POINT('',(-0.195345140381879,-0.000154736422984442,-0.0504796974542436));
#25970=CARTESIAN_POINT('',(-0.195260766042512,-0.000146819403851512,-0.0606536358790897));
#25971=CARTESIAN_POINT('',(-0.1954,-2.39295984553393E-17,-0.19));
#25972=CARTESIAN_POINT('Ctrl Pts',(-0.195345140381879,-0.000154736422984442,
-0.0504796974542436));
#25973=CARTESIAN_POINT('Ctrl Pts',(-0.194969681403942,0.0454695115731484,
-0.0530783631432626));
#25974=CARTESIAN_POINT('Ctrl Pts',(-0.178930944341532,0.0913218023900443,
-0.0556770288322816));
#25975=CARTESIAN_POINT('Ctrl Pts',(-0.149690022397842,0.126037510600571,
-0.0582756945213006));
#25976=CARTESIAN_POINT('Ctrl Pts',(-0.108587064513464,0.174836187169372,
-0.0619285494681118));
#25977=CARTESIAN_POINT('Ctrl Pts',(-0.0413979655074079,0.201630137392092,
-0.065581404414923));
#25978=CARTESIAN_POINT('Ctrl Pts',(0.0219807109386058,0.194462607355388,
-0.0692342593617342));
#25979=CARTESIAN_POINT('Ctrl Pts',(0.0853593873846187,0.187295077318685,
-0.0728871143085453));
#25980=CARTESIAN_POINT('Ctrl Pts',(0.14492764127059,0.146166067022559,-0.0765399692553564));
#25981=CARTESIAN_POINT('Ctrl Pts',(0.174081505004941,0.089422596913196,
-0.0801928242021676));
#25982=CARTESIAN_POINT('Ctrl Pts',(0.203235368739293,0.0326791268038316,
-0.0838456791489788));
#25983=CARTESIAN_POINT('Ctrl Pts',(0.201974842322025,-0.0396788031187714,
-0.08749853409579));
#25984=CARTESIAN_POINT('Ctrl Pts',(0.17088111660692,-0.0953810986953389,
-0.0911513890426013));
#25985=CARTESIAN_POINT('Ctrl Pts',(0.139787390891815,-0.151083394271906,
-0.0948042439894125));
#25986=CARTESIAN_POINT('Ctrl Pts',(0.0788604658788755,-0.190130055502438,
-0.0984570989362236));
#25987=CARTESIAN_POINT('Ctrl Pts',(0.0152639920062928,-0.195105243720415,
-0.102109953883035));
#25988=CARTESIAN_POINT('Ctrl Pts',(-0.04833248186629,-0.200080431938393,
-0.105762808829846));
#25989=CARTESIAN_POINT('Ctrl Pts',(-0.114598504598516,-0.170984147143816,
-0.109415663776657));
#25990=CARTESIAN_POINT('Ctrl Pts',(-0.153974042139665,-0.120793895007844,
-0.113068518723468));
#25991=CARTESIAN_POINT('Ctrl Pts',(-0.180603363641792,-0.0868506794008215,
-0.115538911633727));
#25992=CARTESIAN_POINT('Ctrl Pts',(-0.194933797073887,-0.0432597262598245,
-0.118009304543985));
#25993=CARTESIAN_POINT('Ctrl Pts',(-0.195243803960011,0.00014500399526908,
-0.120479697454244));
#25994=CARTESIAN_POINT('Ctrl Pts',(-0.19528814483522,0.000156602802769957,
-0.13065363587909));
#25995=CARTESIAN_POINT('Ctrl Pts',(-0.194932903946858,-0.0450120911179513,
-0.128081358925247));
#25996=CARTESIAN_POINT('Ctrl Pts',(-0.179288031569788,-0.0904030657414807,
-0.125509081971405));
#25997=CARTESIAN_POINT('Ctrl Pts',(-0.150601799725115,-0.124972231807972,
-0.122936805017562));
#25998=CARTESIAN_POINT('Ctrl Pts',(-0.109864878398407,-0.17406342670613,
-0.119283950070751));
#25999=CARTESIAN_POINT('Ctrl Pts',(-0.042828167949195,-0.20133087817622,
-0.11563109512394));
#26000=CARTESIAN_POINT('Ctrl Pts',(0.0206090388069535,-0.194613033032659,
-0.111978240177129));
#26001=CARTESIAN_POINT('Ctrl Pts',(0.0840462455631022,-0.187895187889097,
-0.108325385230318));
#26002=CARTESIAN_POINT('Ctrl Pts',(0.143883948626187,-0.147192046131885,
-0.104672530283506));
#26003=CARTESIAN_POINT('Ctrl Pts',(0.173435748689723,-0.0906576908474678,
-0.101019675336695));
#26004=CARTESIAN_POINT('Ctrl Pts',(0.202987548753259,-0.03412333556305,
-0.097366820389884));
#26005=CARTESIAN_POINT('Ctrl Pts',(0.202253445817245,0.0382422332485734,
-0.0937139654430728));
#26006=CARTESIAN_POINT('Ctrl Pts',(0.171558198859466,0.0941644594147348,
-0.0900611104962616));
#26007=CARTESIAN_POINT('Ctrl Pts',(0.140862951901687,0.150086685580896,
-0.0864082555494504));
#26008=CARTESIAN_POINT('Ctrl Pts',(0.0802065609221434,0.189565569101596,
-0.0827554006026392));
#26009=CARTESIAN_POINT('Ctrl Pts',(0.0166470195008158,0.194992084644279,
-0.079102545655828));
#26010=CARTESIAN_POINT('Ctrl Pts',(-0.0469125219205106,0.200418600186961,
-0.0754496907090168));
#26011=CARTESIAN_POINT('Ctrl Pts',(-0.113375213783621,0.171792747751628,
-0.0717968357622057));
#26012=CARTESIAN_POINT('Ctrl Pts',(-0.153108187162892,0.121884280074465,
-0.0681439808153946));
#26013=CARTESIAN_POINT('Ctrl Pts',(-0.180266275862396,0.0877710870069687,
-0.0656471991699597));
#26014=CARTESIAN_POINT('Ctrl Pts',(-0.194936428770792,0.0437148063320393,
-0.0631504175245247));
#26015=CARTESIAN_POINT('Ctrl Pts',(-0.195260766042512,-0.000146819403851512,
-0.0606536358790897));
#26016=CARTESIAN_POINT('Origin',(0.,0.,-0.482472289227037));
#26017=CARTESIAN_POINT('',(-0.155506328487213,-0.000123179378687057,-0.0274722892270369));
#26018=CARTESIAN_POINT('',(-0.15555,-6.69085778714157E-17,-0.0253999999999999));
#26019=CARTESIAN_POINT('',(-0.15555,-6.69085778714157E-17,-0.482472289227037));
#26020=CARTESIAN_POINT('',(-0.152866807250001,-0.0287670252405615,-0.0254));
#26021=CARTESIAN_POINT('Ctrl Pts',(-0.155506328487213,-0.000123179378687057,
-0.0274722892270369));
#26022=CARTESIAN_POINT('Ctrl Pts',(-0.155585777160968,-0.00977745909336126,
-0.0267815261513579));
#26023=CARTESIAN_POINT('Ctrl Pts',(-0.154784206338799,-0.0194189119802211,
-0.026090763075679));
#26024=CARTESIAN_POINT('Ctrl Pts',(-0.153064819257014,-0.0288776210951403,
-0.0254));
#26025=CARTESIAN_POINT('Origin',(0.,0.,-0.0254));
#26026=CARTESIAN_POINT('Origin',(0.,0.,-0.482472289227037));
#26027=CARTESIAN_POINT('',(-0.155425658679527,0.000115431788456025,-0.097472289227037));
#26028=CARTESIAN_POINT('',(-0.15543916150416,-0.000116876961459109,-0.0836610441062964));
#26029=CARTESIAN_POINT('',(-0.15555,-6.69085778714157E-17,-0.482472289227037));
#26030=CARTESIAN_POINT('Ctrl Pts',(-0.155425658679527,0.000115431788456041,
-0.097472289227037));
#26031=CARTESIAN_POINT('Ctrl Pts',(-0.155178874794489,-0.0344373102339589,
-0.0950018963167785));
#26032=CARTESIAN_POINT('Ctrl Pts',(-0.126902704468458,-0.120449029386036,
-0.0888786484597088));
#26033=CARTESIAN_POINT('Ctrl Pts',(0.0142761631611888,-0.182438271687888,
-0.0791025456558283));
#26034=CARTESIAN_POINT('Ctrl Pts',(0.159780510946698,-0.0891878906068867,
-0.0681439808153946));
#26035=CARTESIAN_POINT('Ctrl Pts',(0.162790872526117,0.083615732721579,
-0.0571854159749611));
#26036=CARTESIAN_POINT('Ctrl Pts',(0.0205312733659909,0.181839134229702,
-0.0462268511345275));
#26037=CARTESIAN_POINT('Ctrl Pts',(-0.124492415332785,0.124005980435514,
-0.0363224755518862));
#26038=CARTESIAN_POINT('Ctrl Pts',(-0.155207440851501,0.0361964305281632,
-0.0300709549160559));
#26039=CARTESIAN_POINT('Ctrl Pts',(-0.155506328487213,-0.000123179378687057,
-0.0274722892270369));
#26040=CARTESIAN_POINT('',(-0.0768992790589743,0.135212068175182,-0.0253999999999999));
#26041=CARTESIAN_POINT('Origin',(0.,0.,-0.0254));
#26042=CARTESIAN_POINT('Ctrl Pts',(-0.15543916150416,-0.000116876961459117,
-0.0836610441062964));
#26043=CARTESIAN_POINT('Ctrl Pts',(-0.155558710827905,-0.0162840836081317,
-0.0825049708049201));
#26044=CARTESIAN_POINT('Ctrl Pts',(-0.145871418380864,-0.0833967626835857,
-0.0776960425567327));
#26045=CARTESIAN_POINT('Ctrl Pts',(-0.0498103614642923,-0.176085032876655,
-0.069234259361734));
#26046=CARTESIAN_POINT('Ctrl Pts',(0.118915079055016,-0.139024368591976,
-0.0582756945213005));
#26047=CARTESIAN_POINT('Ctrl Pts',(0.18178171708891,0.0219900978007506,
-0.0473171296808669));
#26048=CARTESIAN_POINT('Ctrl Pts',(0.0820716217526228,0.163506105608369,
-0.0363585648404334));
#26049=CARTESIAN_POINT('Ctrl Pts',(-0.0325660146575313,0.160425764828242,
-0.0290528549468111));
#26050=CARTESIAN_POINT('Ctrl Pts',(-0.0768992790589753,0.135212068175181,
-0.0253999999999999));
#26051=CARTESIAN_POINT('Origin',(0.,0.,-0.482472289227037));
#26052=CARTESIAN_POINT('',(-0.155763705058719,-5.51329386419761E-5,-0.167472289227037));
#26053=CARTESIAN_POINT('',(-0.155460956648508,0.00012466512779525,-0.153661044106296));
#26054=CARTESIAN_POINT('',(-0.15555,-6.69085778714157E-17,-0.482472289227037));
#26055=CARTESIAN_POINT('Ctrl Pts',(-0.155763705058719,-5.51329386419977E-5,
-0.167472289227037));
#26056=CARTESIAN_POINT('Ctrl Pts',(-0.155778859312828,-0.00330608558552471,
-0.167238547611123));
#26057=CARTESIAN_POINT('Ctrl Pts',(-0.154228821523255,-0.0573474003148411,
-0.163351951048399));
#26058=CARTESIAN_POINT('Ctrl Pts',(-0.0915954598697826,-0.158421980529086,
-0.155812499538863));
#26059=CARTESIAN_POINT('Ctrl Pts',(0.081145749923459,-0.16402021785595,
-0.144853934698429));
#26060=CARTESIAN_POINT('Ctrl Pts',(0.181504150072734,-0.0233114379958674,
-0.133895369857996));
#26061=CARTESIAN_POINT('Ctrl Pts',(0.119960440554205,0.138191216511648,
-0.122936805017562));
#26062=CARTESIAN_POINT('Ctrl Pts',(-0.0485898940929054,0.176426623792137,
-0.111978240177129));
#26063=CARTESIAN_POINT('Ctrl Pts',(-0.145570304009841,0.0841456530817482,
-0.103490068246954));
#26064=CARTESIAN_POINT('Ctrl Pts',(-0.155543782632231,0.0166542202259733,
-0.0986547512635898));
#26065=CARTESIAN_POINT('Ctrl Pts',(-0.155425658679527,0.000115431788456041,
-0.097472289227037));
#26066=CARTESIAN_POINT('Ctrl Pts',(-0.155460956648508,0.000124665127795244,
-0.153661044106296));
#26067=CARTESIAN_POINT('Ctrl Pts',(-0.155178163812353,-0.0358322966908755,
-0.151088767152454));
#26068=CARTESIAN_POINT('Ctrl Pts',(-0.125037812369975,-0.123279473918762,
-0.1448636352518));
#26069=CARTESIAN_POINT('Ctrl Pts',(0.0192714369799267,-0.181977841230724,
-0.134985648404336));
#26070=CARTESIAN_POINT('Ctrl Pts',(0.162174528762878,-0.0847714896391007,
-0.124027083563902));
#26071=CARTESIAN_POINT('Ctrl Pts',(0.160421360210723,0.0880503767168045,
-0.113068518723468));
#26072=CARTESIAN_POINT('Ctrl Pts',(0.0155630958780523,0.182332981603879,
-0.102109953883035));
#26073=CARTESIAN_POINT('Ctrl Pts',(-0.126416989269986,0.12118136627998,
-0.0923074623439774));
#26074=CARTESIAN_POINT('Ctrl Pts',(-0.155180969781457,0.0347995809874546,
-0.0861578257517313));
#26075=CARTESIAN_POINT('Ctrl Pts',(-0.15543916150416,-0.000116876961459117,
-0.0836610441062964));
#26076=CARTESIAN_POINT('Origin',(0.,0.,-0.482472289227037));
#26077=CARTESIAN_POINT('',(-0.15531970620309,-3.76206267698384E-5,-0.237472289227037));
#26078=CARTESIAN_POINT('',(-0.155738853532286,-7.62666566272302E-5,-0.223661044106296));
#26079=CARTESIAN_POINT('',(-0.15555,-6.69085778714157E-17,-0.482472289227037));
#26080=CARTESIAN_POINT('Ctrl Pts',(-0.15531970620309,-3.76206267698534E-5,
-0.237472289227037));
#26081=CARTESIAN_POINT('Ctrl Pts',(-0.155371303344155,-0.0231547104462748,
-0.235822343958657));
#26082=CARTESIAN_POINT('Ctrl Pts',(-0.139791750558325,-0.0973852770443118,
-0.230519543743466));
#26083=CARTESIAN_POINT('Ctrl Pts',(-0.0260541246753813,-0.181130787616187,
-0.221563888581464));
#26084=CARTESIAN_POINT('Ctrl Pts',(0.136360953114818,-0.122036695554133,
-0.21060532374103));
#26085=CARTESIAN_POINT('Ctrl Pts',(0.177141327667794,0.0459151632427247,
-0.199646758900597));
#26086=CARTESIAN_POINT('Ctrl Pts',(0.0599105989065099,0.172910257764587,
-0.188688194060163));
#26087=CARTESIAN_POINT('Ctrl Pts',(-0.107120389660789,0.146249553923857,
-0.177963370835644));
#26088=CARTESIAN_POINT('Ctrl Pts',(-0.155542032456515,0.0474989814180707,
-0.170891402557935));
#26089=CARTESIAN_POINT('Ctrl Pts',(-0.155763705058719,-5.51329386419977E-5,
-0.167472289227037));
#26090=CARTESIAN_POINT('Ctrl Pts',(-0.155738853532286,-7.62666566272467E-5,
-0.223661044106297));
#26091=CARTESIAN_POINT('Ctrl Pts',(-0.155767412774038,-0.00474623319127167,
-0.223325418446799));
#26092=CARTESIAN_POINT('Ctrl Pts',(-0.153481170317431,-0.0602144763693775,
-0.21933693784049));
#26093=CARTESIAN_POINT('Ctrl Pts',(-0.0872151228846113,-0.160874951949878,
-0.21169560228737));
#26094=CARTESIAN_POINT('Ctrl Pts',(0.0856144901564349,-0.161732502948406,
-0.200737037446937));
#26095=CARTESIAN_POINT('Ctrl Pts',(0.182075453858757,-0.01832367121461,
-0.189778472606503));
#26096=CARTESIAN_POINT('Ctrl Pts',(0.116124144473882,0.141429933431004,
-0.178819907766069));
#26097=CARTESIAN_POINT('Ctrl Pts',(-0.0534107377320515,0.175027279764724,
-0.167861342925636));
#26098=CARTESIAN_POINT('Ctrl Pts',(-0.146691230408257,0.081259908104232,
-0.159475055039045));
#26099=CARTESIAN_POINT('Ctrl Pts',(-0.155579754010068,0.0152296877721218,
-0.154741622099265));
#26100=CARTESIAN_POINT('Ctrl Pts',(-0.155460956648508,0.000124665127795244,
-0.153661044106296));
#26101=CARTESIAN_POINT('Origin',(0.,0.,-0.482472289227037));
#26102=CARTESIAN_POINT('',(-0.155653088469525,0.000125523659554109,-0.307472289227037));
#26103=CARTESIAN_POINT('',(-0.15531185862521,-1.53372867060936E-5,-0.293661044106296));
#26104=CARTESIAN_POINT('',(-0.15555,-6.69085778714157E-17,-0.482472289227037));
#26105=CARTESIAN_POINT('Ctrl Pts',(-0.155653088469525,0.000125523659554115,
-0.307472289227037));
#26106=CARTESIAN_POINT('Ctrl Pts',(-0.155297443306996,-0.0425972855119035,
-0.304406140306191));
#26107=CARTESIAN_POINT('Ctrl Pts',(-0.115130098271041,-0.136833824827096,
-0.297687136438534));
#26108=CARTESIAN_POINT('Ctrl Pts',(0.0432320574545622,-0.177806863527647,
-0.287315277624065));
#26109=CARTESIAN_POINT('Ctrl Pts',(0.171983496481539,-0.0625236655119731,
-0.276356712783632));
#26110=CARTESIAN_POINT('Ctrl Pts',(0.147327574909702,0.10854710720198,-0.265398147943198));
#26111=CARTESIAN_POINT('Ctrl Pts',(-0.00874691461069841,0.182784808841176,
-0.254439583102765));
#26112=CARTESIAN_POINT('Ctrl Pts',(-0.134694247358807,0.107352187029585,
-0.245130963530711));
#26113=CARTESIAN_POINT('Ctrl Pts',(-0.155257071147734,0.0280247907901394,
-0.239475198905468));
#26114=CARTESIAN_POINT('Ctrl Pts',(-0.15531970620309,-3.76206267698534E-5,
-0.237472289227037));
#26115=CARTESIAN_POINT('Ctrl Pts',(-0.15531185862521,-1.5337286706104E-5,
-0.293661044106296));
#26116=CARTESIAN_POINT('Ctrl Pts',(-0.155335373909784,-0.0245633151155352,
-0.291909214794333));
#26117=CARTESIAN_POINT('Ctrl Pts',(-0.138387811535161,-0.100267912744467,
-0.286504530535558));
#26118=CARTESIAN_POINT('Ctrl Pts',(-0.0210751700234872,-0.18177629230341,
-0.277446991329971));
#26119=CARTESIAN_POINT('Ctrl Pts',(0.139657098315878,-0.118250656963312,
-0.266488426489538));
#26120=CARTESIAN_POINT('Ctrl Pts',(0.175815216176257,0.0507574671503514,
-0.255529861649104));
#26121=CARTESIAN_POINT('Ctrl Pts',(0.0551447377802041,0.174488474943397,
-0.244571296808671));
#26122=CARTESIAN_POINT('Ctrl Pts',(-0.109512695395071,0.143552763011982,
-0.233948357627735));
#26123=CARTESIAN_POINT('Ctrl Pts',(-0.155456582047726,0.0460803644623646,
-0.22697827339361));
#26124=CARTESIAN_POINT('Ctrl Pts',(-0.155738853532286,-7.62666566272467E-5,
-0.223661044106297));
#26125=CARTESIAN_POINT('Origin',(2.59090492670967E-17,0.,-0.0254));
#26126=CARTESIAN_POINT('',(0.122919639333555,-0.151894444487311,-0.0254));
#26127=CARTESIAN_POINT('Ctrl Pts',(-0.153064819257014,-0.0288776210951403,
-0.0254));
#26128=CARTESIAN_POINT('Ctrl Pts',(-0.152777592917439,-0.0340072377393832,
-0.0254));
#26129=CARTESIAN_POINT('Ctrl Pts',(-0.152223882228274,-0.0391080712845753,
-0.0254));
#26130=CARTESIAN_POINT('Ctrl Pts',(-0.151399448027242,-0.0441601340310789,
-0.0254));
#26131=CARTESIAN_POINT('Ctrl Pts',(-0.150330370732434,-0.0507113488733025,
-0.0254));
#26132=CARTESIAN_POINT('Ctrl Pts',(-0.14880642391072,-0.0571806323888862,
-0.0253999999999999));
#26133=CARTESIAN_POINT('Ctrl Pts',(-0.146862321130527,-0.063540143599143,
-0.0254));
#26134=CARTESIAN_POINT('Ctrl Pts',(-0.145388672016564,-0.0683607159246997,
-0.0254));
#26135=CARTESIAN_POINT('Ctrl Pts',(-0.143671994693297,-0.0731203555579338,
-0.0253999999999997));
#26136=CARTESIAN_POINT('Ctrl Pts',(-0.141735119284282,-0.0777852836788175,
-0.0253999999999998));
#26137=CARTESIAN_POINT('Ctrl Pts',(-0.138078365687791,-0.0865925061795565,
-0.0253999999999999));
#26138=CARTESIAN_POINT('Ctrl Pts',(-0.133634254588353,-0.0950791659576873,
-0.0253999999999999));
#26139=CARTESIAN_POINT('Ctrl Pts',(-0.128494059306883,-0.103165599018055,
-0.0253999999999999));
#26140=CARTESIAN_POINT('Ctrl Pts',(-0.126025864689144,-0.10704850413418,
-0.0253999999999999));
#26141=CARTESIAN_POINT('Ctrl Pts',(-0.123395149747612,-0.110840498855916,
-0.0253999999999999));
#26142=CARTESIAN_POINT('Ctrl Pts',(-0.120624606677722,-0.114514842153386,
-0.0253999999999999));
#26143=CARTESIAN_POINT('Ctrl Pts',(-0.113588026278536,-0.123846879726758,
-0.0253999999999999));
#26144=CARTESIAN_POINT('Ctrl Pts',(-0.105637653785234,-0.132447744046583,
-0.0253999999999999));
#26145=CARTESIAN_POINT('Ctrl Pts',(-0.0969241262231594,-0.140179311463173,
-0.0253999999999999));
#26146=CARTESIAN_POINT('Ctrl Pts',(-0.09294324074945,-0.14371157600224,
-0.0253999999999999));
#26147=CARTESIAN_POINT('Ctrl Pts',(-0.0888023607437844,-0.147062196487114,
-0.0254));
#26148=CARTESIAN_POINT('Ctrl Pts',(-0.0845127230821876,-0.150216270470207,
-0.0254));
#26149=CARTESIAN_POINT('Ctrl Pts',(-0.0807618339747387,-0.152974214772399,
-0.0254));
#26150=CARTESIAN_POINT('Ctrl Pts',(-0.0768933726595271,-0.155583707402879,
-0.0253999999999999));
#26151=CARTESIAN_POINT('Ctrl Pts',(-0.0729386575525788,-0.158019936339133,
-0.0253999999999999));
#26152=CARTESIAN_POINT('Ctrl Pts',(-0.0664307842915506,-0.162028991030365,
-0.0253999999999999));
#26153=CARTESIAN_POINT('Ctrl Pts',(-0.0596792629904233,-0.165577918385484,
-0.0253999999999999));
#26154=CARTESIAN_POINT('Ctrl Pts',(-0.0527219813591869,-0.168628838889641,
-0.0253999999999999));
#26155=CARTESIAN_POINT('Ctrl Pts',(-0.0455901588913395,-0.17175629937672,
-0.0254));
#26156=CARTESIAN_POINT('Ctrl Pts',(-0.0382420298855482,-0.174360754422375,
-0.0254));
#26157=CARTESIAN_POINT('Ctrl Pts',(-0.0307291264526019,-0.176457918562462,
-0.0254));
#26158=CARTESIAN_POINT('Ctrl Pts',(-0.0265471472130843,-0.177625283080584,
-0.0254));
#26159=CARTESIAN_POINT('Ctrl Pts',(-0.0223140014545879,-0.178635304140707,
-0.0253999999999999));
#26160=CARTESIAN_POINT('Ctrl Pts',(-0.0180379599774122,-0.179489460836271,
-0.0253999999999999));
#26161=CARTESIAN_POINT('Ctrl Pts',(-0.0145498200543281,-0.180186230988354,
-0.0253999999999999));
#26162=CARTESIAN_POINT('Ctrl Pts',(-0.0110380948897776,-0.180778117133158,
-0.0254000000000001));
#26163=CARTESIAN_POINT('Ctrl Pts',(-0.0075153478077699,-0.181265734494698,
-0.0254000000000001));
#26164=CARTESIAN_POINT('Ctrl Pts',(0.00372069158298919,-0.182821022954056,
-0.0254));
#26165=CARTESIAN_POINT('Ctrl Pts',(0.0150906888787215,-0.183322996861398,
-0.0254));
#26166=CARTESIAN_POINT('Ctrl Pts',(0.0264435674523557,-0.182817859387596,
-0.0254));
#26167=CARTESIAN_POINT('Ctrl Pts',(0.0340855280180532,-0.182477836315033,
-0.0254000000000001));
#26168=CARTESIAN_POINT('Ctrl Pts',(0.0417202563974908,-0.181680756711447,
-0.0254));
#26169=CARTESIAN_POINT('Ctrl Pts',(0.0493042471779824,-0.180431503266826,
-0.0254));
#26170=CARTESIAN_POINT('Ctrl Pts',(0.0532122465331841,-0.17978776808869,
-0.0254));
#26171=CARTESIAN_POINT('Ctrl Pts',(0.0571088690032366,-0.179023120919283,
-0.0254));
#26172=CARTESIAN_POINT('Ctrl Pts',(0.0609702128695543,-0.178142282480996,
-0.0254));
#26173=CARTESIAN_POINT('Ctrl Pts',(0.0734785721675836,-0.175288912242277,
-0.0254000000000001));
#26174=CARTESIAN_POINT('Ctrl Pts',(0.0856546858321524,-0.171215349953341,
-0.0254));
#26175=CARTESIAN_POINT('Ctrl Pts',(0.0973011784066163,-0.165963075675207,
-0.0254));
#26176=CARTESIAN_POINT('Ctrl Pts',(0.106177882671306,-0.161959906035425,
-0.0254));
#26177=CARTESIAN_POINT('Ctrl Pts',(0.114747547478628,-0.157270963555419,
-0.0254));
#26178=CARTESIAN_POINT('Ctrl Pts',(0.122919639333555,-0.151894444487311,
-0.0254));
#26179=CARTESIAN_POINT('',(-0.1954,-2.39295984553393E-17,-0.0254));
#26180=CARTESIAN_POINT('Origin',(0.,0.,-0.0254));
#26181=CARTESIAN_POINT('',(0.195483386661889,0.00449643670064488,-0.0254));
#26182=CARTESIAN_POINT('Origin',(0.,0.,-0.0254));
#26183=CARTESIAN_POINT('Ctrl Pts',(0.1956174094926,0.00454472201517893,
-0.0254));
#26184=CARTESIAN_POINT('Ctrl Pts',(0.194884502242902,0.0108609228279264,
-0.0254));
#26185=CARTESIAN_POINT('Ctrl Pts',(0.193827694703694,0.0171246191869846,
-0.0254));
#26186=CARTESIAN_POINT('Ctrl Pts',(0.192436221146521,0.0233138906391813,
-0.0254));
#26187=CARTESIAN_POINT('Ctrl Pts',(0.190305921538478,0.0327894588098559,
-0.0254));
#26188=CARTESIAN_POINT('Ctrl Pts',(0.187391725008866,0.0420911964277299,
-0.0254000000000001));
#26189=CARTESIAN_POINT('Ctrl Pts',(0.183750788578834,0.0511458524301873,
-0.0254000000000001));
#26190=CARTESIAN_POINT('Ctrl Pts',(0.182256333478902,0.0548624174131394,
-0.0254000000000001));
#26191=CARTESIAN_POINT('Ctrl Pts',(0.180639878796232,0.0585352549444029,
-0.0254));
#26192=CARTESIAN_POINT('Ctrl Pts',(0.178909447829662,0.0621511985197291,
-0.0254));
#26193=CARTESIAN_POINT('Ctrl Pts',(0.175759243024173,0.0687339302480849,
-0.0254));
#26194=CARTESIAN_POINT('Ctrl Pts',(0.172228441682624,0.0751362936533435,
-0.0254));
#26195=CARTESIAN_POINT('Ctrl Pts',(0.168341962135569,0.081327087720111,
-0.0254000000000001));
#26196=CARTESIAN_POINT('Ctrl Pts',(0.165097336199203,0.0864954697359009,
-0.0254000000000001));
#26197=CARTESIAN_POINT('Ctrl Pts',(0.161604700724613,0.0915163594823662,
-0.0254000000000001));
#26198=CARTESIAN_POINT('Ctrl Pts',(0.157876721750264,0.0963691400874196,
-0.0254000000000002));
#26199=CARTESIAN_POINT('Ctrl Pts',(0.155393249616941,0.0996019226445926,
-0.0254000000000002));
#26200=CARTESIAN_POINT('Ctrl Pts',(0.152811199634149,0.102752305844702,
-0.0254));
#26201=CARTESIAN_POINT('Ctrl Pts',(0.15013686171718,0.105813287041844,-0.0254));
#26202=CARTESIAN_POINT('Ctrl Pts',(0.142106471379143,0.115004673692902,
-0.0254));
#26203=CARTESIAN_POINT('Ctrl Pts',(0.133241108450999,0.123399305600953,
-0.0254));
#26204=CARTESIAN_POINT('Ctrl Pts',(0.123649781692531,0.130835395348286,
-0.0254000000000001));
#26205=CARTESIAN_POINT('Ctrl Pts',(0.119112362619058,0.134353225185729,
-0.0254000000000001));
#26206=CARTESIAN_POINT('Ctrl Pts',(0.114412125674294,0.137655883629633,
-0.0253999999999999));
#26207=CARTESIAN_POINT('Ctrl Pts',(0.109559388770948,0.140722179479723,
-0.0253999999999999));
#26208=CARTESIAN_POINT('Ctrl Pts',(0.106359640552875,0.14274400239694,-0.0253999999999999));
#26209=CARTESIAN_POINT('Ctrl Pts',(0.103091731428373,0.144663720869763,
-0.0254));
#26210=CARTESIAN_POINT('Ctrl Pts',(0.0997741086716124,0.146466938326076,
-0.0254));
#26211=CARTESIAN_POINT('Ctrl Pts',(0.0929232199256937,0.150190581152171,
-0.0254));
#26212=CARTESIAN_POINT('Ctrl Pts',(0.0858475401072859,0.153427047025761,
-0.0254));
#26213=CARTESIAN_POINT('Ctrl Pts',(0.078575952192563,0.156129623366496,
-0.0254));
#26214=CARTESIAN_POINT('Ctrl Pts',(0.0721329233957311,0.158524255377166,
-0.0254));
#26215=CARTESIAN_POINT('Ctrl Pts',(0.0655359016892521,0.160499536766023,
-0.0254));
#26216=CARTESIAN_POINT('Ctrl Pts',(0.0588237208555869,0.162058462470114,
-0.0254));
#26217=CARTESIAN_POINT('Ctrl Pts',(0.0538349286583048,0.163217125590407,
-0.0254));
#26218=CARTESIAN_POINT('Ctrl Pts',(0.0487825015420083,0.164145657243952,
-0.0254));
#26219=CARTESIAN_POINT('Ctrl Pts',(0.0436829085690683,0.164843212472954,
-0.0254));
#26220=CARTESIAN_POINT('Ctrl Pts',(0.039963114449189,0.165352029912483,
-0.0254));
#26221=CARTESIAN_POINT('Ctrl Pts',(0.0362254315579577,0.165736782759396,
-0.0254));
#26222=CARTESIAN_POINT('Ctrl Pts',(0.0324835004058875,0.165997995639231,
-0.0254));
#26223=CARTESIAN_POINT('Ctrl Pts',(0.0228345603237951,0.1666715589208,-0.0254000000000001));
#26224=CARTESIAN_POINT('Ctrl Pts',(0.0131416919040143,0.166527582794073,
-0.0254));
#26225=CARTESIAN_POINT('Ctrl Pts',(0.00351603350894282,0.165574729310518,
-0.0254));
#26226=CARTESIAN_POINT('Ctrl Pts',(-0.00271730357169677,0.164957685082718,
-0.0253999999999999));
#26227=CARTESIAN_POINT('Ctrl Pts',(-0.00892239601177496,0.164000905828904,
-0.0254));
#26228=CARTESIAN_POINT('Ctrl Pts',(-0.0150663391055822,0.16270149682046,
-0.0254000000000001));
#26229=CARTESIAN_POINT('Ctrl Pts',(-0.0195365657371929,0.161756069321179,
-0.0254000000000001));
#26230=CARTESIAN_POINT('Ctrl Pts',(-0.0239783961275451,0.160627551616827,
-0.0253999999999999));
#26231=CARTESIAN_POINT('Ctrl Pts',(-0.0283517173245239,0.159322701788556,
-0.0254));
#26232=CARTESIAN_POINT('Ctrl Pts',(-0.0386808148966284,0.156240851499933,
-0.0254));
#26233=CARTESIAN_POINT('Ctrl Pts',(-0.0486583234698455,0.15217404561927,
-0.0254000000000001));
#26234=CARTESIAN_POINT('Ctrl Pts',(-0.0581163771297697,0.147117423395272,
-0.0254));
#26235=CARTESIAN_POINT('Ctrl Pts',(-0.0646475390281869,0.143625624808423,
-0.0254));
#26236=CARTESIAN_POINT('Ctrl Pts',(-0.0709305950931194,0.139660961676877,
-0.0254));
#26237=CARTESIAN_POINT('Ctrl Pts',(-0.0768992790589734,0.135212068175182,
-0.0254));
#26238=CARTESIAN_POINT('Ctrl Pts',(-0.0685825729128703,0.139614588036676,
-0.376074074893873));
#26239=CARTESIAN_POINT('Ctrl Pts',(-0.114359333295748,0.117127768780733,
-0.372421219947062));
#26240=CARTESIAN_POINT('Ctrl Pts',(-0.181359531123569,0.0240565612455276,
-0.36511551005344));
#26241=CARTESIAN_POINT('Ctrl Pts',(-0.12038866893656,-0.137966392504705,
-0.354156945213007));
#26242=CARTESIAN_POINT('Ctrl Pts',(0.0481126911101254,-0.176504221035079,
-0.343198380372572));
#26243=CARTESIAN_POINT('Ctrl Pts',(0.173623780493455,-0.0578082499262578,
-0.332239815532139));
#26244=CARTESIAN_POINT('Ctrl Pts',(0.144299756757966,0.112561276791376,
-0.321281250691706));
#26245=CARTESIAN_POINT('Ctrl Pts',(-0.0137605119892857,0.182468951639323,
-0.310322685851272));
#26246=CARTESIAN_POINT('Ctrl Pts',(-0.159535841690899,0.0896428544271446,
-0.299364121010838));
#26247=CARTESIAN_POINT('Ctrl Pts',(-0.16300976830989,-0.0831606703158766,
-0.288405556170405));
#26248=CARTESIAN_POINT('Ctrl Pts',(-0.0210751700234872,-0.18177629230341,
-0.277446991329971));
#26249=CARTESIAN_POINT('Ctrl Pts',(0.139657098315878,-0.118250656963312,
-0.266488426489538));
#26250=CARTESIAN_POINT('Ctrl Pts',(0.175815216176257,0.0507574671503514,
-0.255529861649104));
#26251=CARTESIAN_POINT('Ctrl Pts',(0.0551447377802041,0.174488474943397,
-0.244571296808671));
#26252=CARTESIAN_POINT('Ctrl Pts',(-0.114714952384342,0.14257536696912,
-0.233612731968237));
#26253=CARTESIAN_POINT('Ctrl Pts',(-0.182248350055914,-0.0165161103770323,
-0.222654167127804));
#26254=CARTESIAN_POINT('Ctrl Pts',(-0.0872151228846113,-0.160874951949878,
-0.21169560228737));
#26255=CARTESIAN_POINT('Ctrl Pts',(0.0856144901564349,-0.161732502948406,
-0.200737037446937));
#26256=CARTESIAN_POINT('Ctrl Pts',(0.182075453858757,-0.01832367121461,
-0.189778472606503));
#26257=CARTESIAN_POINT('Ctrl Pts',(0.116124144473882,0.141429933431004,
-0.178819907766069));
#26258=CARTESIAN_POINT('Ctrl Pts',(-0.0534107377320515,0.175027279764724,
-0.167861342925636));
#26259=CARTESIAN_POINT('Ctrl Pts',(-0.175302609459258,0.0524991915146761,
-0.156902778085202));
#26260=CARTESIAN_POINT('Ctrl Pts',(-0.140824166557048,-0.116858310890308,
-0.145944213244769));
#26261=CARTESIAN_POINT('Ctrl Pts',(0.0192714369799267,-0.181977841230724,
-0.134985648404336));
#26262=CARTESIAN_POINT('Ctrl Pts',(0.162174528762878,-0.0847714896391007,
-0.124027083563902));
#26263=CARTESIAN_POINT('Ctrl Pts',(0.160421360210723,0.0880503767168045,
-0.113068518723468));
#26264=CARTESIAN_POINT('Ctrl Pts',(0.0155630958780523,0.182332981603879,
-0.102109953883035));
#26265=CARTESIAN_POINT('Ctrl Pts',(-0.143161649044776,0.113969347832393,
-0.0911513890426012));
#26266=CARTESIAN_POINT('Ctrl Pts',(-0.174215737565518,-0.0560476370404291,
-0.0801928242021676));
#26267=CARTESIAN_POINT('Ctrl Pts',(-0.0498103614642923,-0.176085032876655,
-0.069234259361734));
#26268=CARTESIAN_POINT('Ctrl Pts',(0.118915079055016,-0.139024368591976,
-0.0582756945213005));
#26269=CARTESIAN_POINT('Ctrl Pts',(0.18178171708891,0.0219900978007506,
-0.0473171296808669));
#26270=CARTESIAN_POINT('Ctrl Pts',(0.0820716217526228,0.163506105608369,
-0.0363585648404334));
#26271=CARTESIAN_POINT('Ctrl Pts',(-0.0325660146575313,0.160425764828242,
-0.0290528549468111));
#26272=CARTESIAN_POINT('Ctrl Pts',(-0.0768992790589753,0.135212068175181,
-0.0253999999999999));
#26273=CARTESIAN_POINT('Ctrl Pts',(-0.0744392439309307,0.151537102412036,
-0.368404938818138));
#26274=CARTESIAN_POINT('Ctrl Pts',(-0.124125152286074,0.127130000830261,
-0.364752083871327));
#26275=CARTESIAN_POINT('Ctrl Pts',(-0.196846892776358,0.0261108931123106,
-0.357446373977704));
#26276=CARTESIAN_POINT('Ctrl Pts',(-0.13066936851252,-0.149748157727705,
-0.34648780913727));
#26277=CARTESIAN_POINT('Ctrl Pts',(0.0522213180055256,-0.191576959079111,
-0.335529244296837));
#26278=CARTESIAN_POINT('Ctrl Pts',(0.188450540704886,-0.0627448378606012,
-0.324570679456403));
#26279=CARTESIAN_POINT('Ctrl Pts',(0.156622365365713,0.12217354911568,-0.31361211461597));
#26280=CARTESIAN_POINT('Ctrl Pts',(-0.0149356033913493,0.198051053263296,
-0.302653549775536));
#26281=CARTESIAN_POINT('Ctrl Pts',(-0.173159549590572,0.0972979872867219,
-0.291694984935103));
#26282=CARTESIAN_POINT('Ctrl Pts',(-0.176930135324031,-0.0902622511839527,
-0.280736420094669));
#26283=CARTESIAN_POINT('Ctrl Pts',(-0.0228749032827522,-0.197299243655153,
-0.269777855254236));
#26284=CARTESIAN_POINT('Ctrl Pts',(0.151583242895087,-0.128348779067647,
-0.258819290413802));
#26285=CARTESIAN_POINT('Ctrl Pts',(0.190829116025446,0.0550919470945095,
-0.247860725573369));
#26286=CARTESIAN_POINT('Ctrl Pts',(0.0598538726790387,0.189389076521656,
-0.236902160732935));
#26287=CARTESIAN_POINT('Ctrl Pts',(-0.124511139789284,0.154750719746832,
-0.225943595892502));
#26288=CARTESIAN_POINT('Ctrl Pts',(-0.197811613207586,-0.0179265186027361,
-0.214985031052068));
#26289=CARTESIAN_POINT('Ctrl Pts',(-0.0946629374071695,-0.174613014384685,
-0.204026466211635));
#26290=CARTESIAN_POINT('Ctrl Pts',(0.092925617195402,-0.175543796728528,
-0.193067901371201));
#26291=CARTESIAN_POINT('Ctrl Pts',(0.197623952382857,-0.0198884377374904,
-0.182109336530767));
#26292=CARTESIAN_POINT('Ctrl Pts',(0.126040671115443,0.153507470872824,
-0.171150771690334));
#26293=CARTESIAN_POINT('Ctrl Pts',(-0.0579717961240417,0.189973893069395,
-0.1601922068499));
#26294=CARTESIAN_POINT('Ctrl Pts',(-0.190272734792916,0.0569824075906642,
-0.149233642009467));
#26295=CARTESIAN_POINT('Ctrl Pts',(-0.152849973987239,-0.126837532338885,
-0.138275077169033));
#26296=CARTESIAN_POINT('Ctrl Pts',(0.0209171388199568,-0.197518004035919,
-0.1273165123286));
#26297=CARTESIAN_POINT('Ctrl Pts',(0.176023569738343,-0.0920106278842914,
-0.116357947488166));
#26298=CARTESIAN_POINT('Ctrl Pts',(0.174120687767559,0.0955695184979354,
-0.105399382647733));
#26299=CARTESIAN_POINT('Ctrl Pts',(0.0168921205662348,0.197903471943351,
-0.0944408178072992));
#26300=CARTESIAN_POINT('Ctrl Pts',(-0.155387067912095,0.123701863660361,
-0.0834822529668656));
#26301=CARTESIAN_POINT('Ctrl Pts',(-0.18909304848802,-0.0608338758405172,
-0.0725236881264321));
#26302=CARTESIAN_POINT('Ctrl Pts',(-0.0540639624593679,-0.191121973967697,
-0.0615651232859985));
#26303=CARTESIAN_POINT('Ctrl Pts',(0.129069940086501,-0.150896480642528,
-0.050606558445565));
#26304=CARTESIAN_POINT('Ctrl Pts',(0.197305131695131,0.0238679621473913,
-0.0396479936051314));
#26305=CARTESIAN_POINT('Ctrl Pts',(0.0890802023308762,0.17746885779629,
-0.0286894287646979));
#26306=CARTESIAN_POINT('Ctrl Pts',(-0.0353470190164783,0.174125468521385,
-0.0213837188710755));
#26307=CARTESIAN_POINT('Ctrl Pts',(-0.0834661627416072,0.146758625373897,
-0.0177308639242643));
#26308=CARTESIAN_POINT('Ctrl Pts',(-0.0802959149489911,0.163459616787395,
-0.360735802742402));
#26309=CARTESIAN_POINT('Ctrl Pts',(-0.1338909712764,0.137132232879789,-0.357082947795591));
#26310=CARTESIAN_POINT('Ctrl Pts',(-0.212334254429148,0.0281652249790934,
-0.349777237901969));
#26311=CARTESIAN_POINT('Ctrl Pts',(-0.140950068088481,-0.161529922950703,
-0.338818673061535));
#26312=CARTESIAN_POINT('Ctrl Pts',(0.0563299449009258,-0.206649697123144,
-0.327860108221102));
#26313=CARTESIAN_POINT('Ctrl Pts',(0.203277300916317,-0.0676814257949445,
-0.316901543380668));
#26314=CARTESIAN_POINT('Ctrl Pts',(0.168944973973459,0.131785821439984,
-0.305942978540234));
#26315=CARTESIAN_POINT('Ctrl Pts',(-0.016110694793413,0.213633154887269,
-0.294984413699801));
#26316=CARTESIAN_POINT('Ctrl Pts',(-0.186783257490245,0.104953120146299,
-0.284025848859367));
#26317=CARTESIAN_POINT('Ctrl Pts',(-0.190850502338172,-0.0973638320520286,
-0.273067284018934));
#26318=CARTESIAN_POINT('Ctrl Pts',(-0.0246746365420171,-0.212822195006897,
-0.2621087191785));
#26319=CARTESIAN_POINT('Ctrl Pts',(0.163509387474296,-0.138446901171982,
-0.251150154338067));
#26320=CARTESIAN_POINT('Ctrl Pts',(0.205843015874634,0.0594264270386681,
-0.240191589497633));
#26321=CARTESIAN_POINT('Ctrl Pts',(0.0645630075778731,0.204289678099914,
-0.2292330246572));
#26322=CARTESIAN_POINT('Ctrl Pts',(-0.134307327194226,0.166926072524544,
-0.218274459816766));
#26323=CARTESIAN_POINT('Ctrl Pts',(-0.213374876359259,-0.0193369268284401,
-0.207315894976333));
#26324=CARTESIAN_POINT('Ctrl Pts',(-0.102110751929727,-0.188351076819492,
-0.196357330135899));
#26325=CARTESIAN_POINT('Ctrl Pts',(0.100236744234369,-0.18935509050865,
-0.185398765295466));
#26326=CARTESIAN_POINT('Ctrl Pts',(0.213172450906958,-0.0214532042603709,
-0.174440200455032));
#26327=CARTESIAN_POINT('Ctrl Pts',(0.135957197757003,0.165585008314644,
-0.163481635614599));
#26328=CARTESIAN_POINT('Ctrl Pts',(-0.062532854516032,0.204920506374065,
-0.152523070774164));
#26329=CARTESIAN_POINT('Ctrl Pts',(-0.205242860126574,0.0614656236666522,
-0.141564505933732));
#26330=CARTESIAN_POINT('Ctrl Pts',(-0.164875781417429,-0.136816753787463,
-0.130605941093298));
#26331=CARTESIAN_POINT('Ctrl Pts',(0.0225628406599869,-0.213058166841115,
-0.119647376252864));
#26332=CARTESIAN_POINT('Ctrl Pts',(0.189872610713808,-0.0992497661294819,
-0.108688811412431));
#26333=CARTESIAN_POINT('Ctrl Pts',(0.187820015324394,0.103088660279066,
-0.0977302465719972));
#26334=CARTESIAN_POINT('Ctrl Pts',(0.0182211452544175,0.213473962282823,
-0.0867716817315636));
#26335=CARTESIAN_POINT('Ctrl Pts',(-0.167612486779414,0.133434379488328,
-0.0758131168911301));
#26336=CARTESIAN_POINT('Ctrl Pts',(-0.203970359410523,-0.0656201146406053,
-0.0648545520506966));
#26337=CARTESIAN_POINT('Ctrl Pts',(-0.0583175634544437,-0.206158915058739,
-0.0538959872102629));
#26338=CARTESIAN_POINT('Ctrl Pts',(0.139224801117986,-0.162768592693081,
-0.0429374223698294));
#26339=CARTESIAN_POINT('Ctrl Pts',(0.212828546301352,0.025745826494032,
-0.0319788575293959));
#26340=CARTESIAN_POINT('Ctrl Pts',(0.0960887829091298,0.191431609984211,
-0.0210202926889623));
#26341=CARTESIAN_POINT('Ctrl Pts',(-0.0381280233754254,0.187825172214529,
-0.01371458279534));
#26342=CARTESIAN_POINT('Ctrl Pts',(-0.090033046424239,0.158305182572614,
-0.0100617278485288));
#26343=CARTESIAN_POINT('Ctrl Pts',(-0.0861525859670515,0.175382131162755,
-0.353066666666667));
#26344=CARTESIAN_POINT('Ctrl Pts',(-0.143656790266726,0.147134464929317,
-0.349413811719856));
#26345=CARTESIAN_POINT('Ctrl Pts',(-0.227821616081937,0.0302195568458765,
-0.342108101826233));
#26346=CARTESIAN_POINT('Ctrl Pts',(-0.151230767664441,-0.173311688173703,
-0.3311495369858));
#26347=CARTESIAN_POINT('Ctrl Pts',(0.0604385717963258,-0.221722435167177,
-0.320190972145366));
#26348=CARTESIAN_POINT('Ctrl Pts',(0.218104061127748,-0.072618013729288,
-0.309232407304933));
#26349=CARTESIAN_POINT('Ctrl Pts',(0.181267582581206,0.141398093764287,
-0.298273842464499));
#26350=CARTESIAN_POINT('Ctrl Pts',(-0.0172857861954766,0.229215256511242,
-0.287315277624066));
#26351=CARTESIAN_POINT('Ctrl Pts',(-0.200406965389918,0.112608253005876,
-0.276356712783632));
#26352=CARTESIAN_POINT('Ctrl Pts',(-0.204770869352314,-0.104465412920104,
-0.265398147943198));
#26353=CARTESIAN_POINT('Ctrl Pts',(-0.0264743698012821,-0.22834514635864,
-0.254439583102765));
#26354=CARTESIAN_POINT('Ctrl Pts',(0.175435532053505,-0.148545023276317,
-0.243481018262331));
#26355=CARTESIAN_POINT('Ctrl Pts',(0.220856915723823,0.0637609069828263,
-0.232522453421897));
#26356=CARTESIAN_POINT('Ctrl Pts',(0.0692721424767077,0.219190279678173,
-0.221563888581465));
#26357=CARTESIAN_POINT('Ctrl Pts',(-0.144103514599168,0.179101425302256,
-0.21060532374103));
#26358=CARTESIAN_POINT('Ctrl Pts',(-0.228938139510932,-0.0207473350541439,
-0.199646758900597));
#26359=CARTESIAN_POINT('Ctrl Pts',(-0.109558566452286,-0.202089139254299,
-0.188688194060163));
#26360=CARTESIAN_POINT('Ctrl Pts',(0.107547871273336,-0.203166384288772,
-0.17772962921973));
#26361=CARTESIAN_POINT('Ctrl Pts',(0.228720949431058,-0.0230179707832516,
-0.166771064379296));
#26362=CARTESIAN_POINT('Ctrl Pts',(0.145873724398564,0.177662545756465,
-0.155812499538863));
#26363=CARTESIAN_POINT('Ctrl Pts',(-0.0670939129080224,0.219867119678735,
-0.144853934698429));
#26364=CARTESIAN_POINT('Ctrl Pts',(-0.220212985460232,0.0659488397426404,
-0.133895369857996));
#26365=CARTESIAN_POINT('Ctrl Pts',(-0.17690158884762,-0.146795975236041,
-0.122936805017562));
#26366=CARTESIAN_POINT('Ctrl Pts',(0.024208542500017,-0.22859832964631,
-0.111978240177129));
#26367=CARTESIAN_POINT('Ctrl Pts',(0.203721651689273,-0.106488904374672,
-0.101019675336695));
#26368=CARTESIAN_POINT('Ctrl Pts',(0.20151934288123,0.110607802060197,-0.0900611104962616));
#26369=CARTESIAN_POINT('Ctrl Pts',(0.0195501699426001,0.229044452622295,
-0.079102545655828));
#26370=CARTESIAN_POINT('Ctrl Pts',(-0.179837905646733,0.143166895316295,
-0.0681439808153946));
#26371=CARTESIAN_POINT('Ctrl Pts',(-0.218847670333026,-0.0704063534406933,
-0.0571854159749609));
#26372=CARTESIAN_POINT('Ctrl Pts',(-0.0625711644495193,-0.221195856149781,
-0.0462268511345275));
#26373=CARTESIAN_POINT('Ctrl Pts',(0.149379662149471,-0.174640704743633,
-0.0352682862940938));
#26374=CARTESIAN_POINT('Ctrl Pts',(0.228351960907573,0.0276236908406728,
-0.0243097214536604));
#26375=CARTESIAN_POINT('Ctrl Pts',(0.103097363487383,0.205394362172133,
-0.0133511566132268));
#26376=CARTESIAN_POINT('Ctrl Pts',(-0.0409090277343724,0.201524875907672,
-0.00604544671960447));
#26377=CARTESIAN_POINT('Ctrl Pts',(-0.0965999301068709,0.16985173977133,
-0.00239259177279327));
#26378=CARTESIAN_POINT('Ctrl Pts',(-0.195260766042512,-0.000146819403851512,
-0.0606536358790897));
#26379=CARTESIAN_POINT('Ctrl Pts',(-0.195410942435055,-0.0204558658761102,
-0.0594975625777135));
#26380=CARTESIAN_POINT('Ctrl Pts',(-0.192485483346375,-0.0407231797866054,
-0.0583414892763372));
#26381=CARTESIAN_POINT('Ctrl Pts',(-0.186299958571393,-0.0599423957660427,
-0.057185415974961));
#26382=CARTESIAN_POINT('Ctrl Pts',(-0.16675550170519,-0.120669521010389,
-0.0535325610281498));
#26383=CARTESIAN_POINT('Ctrl Pts',(-0.114663333077355,-0.170932688580085,
-0.0498797060813386));
#26384=CARTESIAN_POINT('Ctrl Pts',(-0.0532921109969387,-0.188305080463908,
-0.0462268511345274));
#26385=CARTESIAN_POINT('Ctrl Pts',(0.00807911108347766,-0.205677472347732,
-0.0425739961877162));
#26386=CARTESIAN_POINT('Ctrl Pts',(0.0787293866164743,-0.190159088545682,
-0.038921141240905));
#26387=CARTESIAN_POINT('Ctrl Pts',(0.12721657417599,-0.148689164047273,
-0.0352682862940938));
#26388=CARTESIAN_POINT('Ctrl Pts',(0.170879723082794,-0.11134512370042,
-0.0319788575293959));
#26389=CARTESIAN_POINT('Ctrl Pts',(0.196570459065126,-0.0529565517441027,
-0.0286894287646979));
#26390=CARTESIAN_POINT('Ctrl Pts',(0.1956174094926,0.00454472201517893,
-0.0254));
#26391=CARTESIAN_POINT('',(-0.090544221732454,-0.126745838915641,-0.353066666666667));
#26392=CARTESIAN_POINT('Ctrl Pts',(-0.0905442217324535,-0.126745838915641,
-0.353066666666667));
#26393=CARTESIAN_POINT('Ctrl Pts',(-0.0950778866087321,-0.124328949845596,
-0.353066666666667));
#26394=CARTESIAN_POINT('Ctrl Pts',(-0.0994734168556016,-0.121682361637407,
-0.353066666666667));
#26395=CARTESIAN_POINT('Ctrl Pts',(-0.103710894594221,-0.118810629553691,
-0.353066666666667));
#26396=CARTESIAN_POINT('Ctrl Pts',(-0.109205802656033,-0.115086738892423,
-0.353066666666667));
#26397=CARTESIAN_POINT('Ctrl Pts',(-0.114435163201789,-0.110984556163928,
-0.353066666666667));
#26398=CARTESIAN_POINT('Ctrl Pts',(-0.119388306282607,-0.106547282912304,
-0.353066666666667));
#26399=CARTESIAN_POINT('Ctrl Pts',(-0.123142837628399,-0.103183785988989,
-0.353066666666667));
#26400=CARTESIAN_POINT('Ctrl Pts',(-0.126739923081413,-0.0996253876790819,
-0.353066666666667));
#26401=CARTESIAN_POINT('Ctrl Pts',(-0.130158509803707,-0.0959070026082769,
-0.353066666666667));
#26402=CARTESIAN_POINT('Ctrl Pts',(-0.136612470751906,-0.0888870513866671,
-0.353066666666667));
#26403=CARTESIAN_POINT('Ctrl Pts',(-0.142444637276161,-0.0812874705536567,
-0.353066666666667));
#26404=CARTESIAN_POINT('Ctrl Pts',(-0.147621095756717,-0.0732245560109258,
-0.353066666666667));
#26405=CARTESIAN_POINT('Ctrl Pts',(-0.150106918494648,-0.0693526083502609,
-0.353066666666667));
#26406=CARTESIAN_POINT('Ctrl Pts',(-0.152441921172652,-0.0653713975830042,
-0.353066666666667));
#26407=CARTESIAN_POINT('Ctrl Pts',(-0.15461137646505,-0.0613127594075525,
-0.353066666666667));
#26408=CARTESIAN_POINT('Ctrl Pts',(-0.160121027420107,-0.051005250523656,
-0.353066666666667));
#26409=CARTESIAN_POINT('Ctrl Pts',(-0.164583123630244,-0.0401759575950903,
-0.353066666666667));
#26410=CARTESIAN_POINT('Ctrl Pts',(-0.167935657633854,-0.0290196273550922,
-0.353066666666667));
#26411=CARTESIAN_POINT('Ctrl Pts',(-0.169467297684012,-0.0239227417783969,
-0.353066666666667));
#26412=CARTESIAN_POINT('Ctrl Pts',(-0.17076686879121,-0.0187570404330206,
-0.353066666666667));
#26413=CARTESIAN_POINT('Ctrl Pts',(-0.171825572631564,-0.0135389836432372,
-0.353066666666667));
#26414=CARTESIAN_POINT('Ctrl Pts',(-0.172751335094915,-0.00897615792797176,
-0.353066666666667));
#26415=CARTESIAN_POINT('Ctrl Pts',(-0.17349296837949,-0.00436905326050375,
-0.353066666666667));
#26416=CARTESIAN_POINT('Ctrl Pts',(-0.174041123319537,0.000243481210159243,
-0.353066666666667));
#26417=CARTESIAN_POINT('Ctrl Pts',(-0.174943147920424,0.00783370663915697,
-0.353066666666667));
#26418=CARTESIAN_POINT('Ctrl Pts',(-0.175325250731135,0.0154515874573274,
-0.353066666666667));
#26419=CARTESIAN_POINT('Ctrl Pts',(-0.175168987402103,0.0230468219305827,
-0.353066666666667));
#26420=CARTESIAN_POINT('Ctrl Pts',(-0.175008803924067,0.0308325966350812,
-0.353066666666667));
#26421=CARTESIAN_POINT('Ctrl Pts',(-0.174283139083255,0.0385947856858029,
-0.353066666666667));
#26422=CARTESIAN_POINT('Ctrl Pts',(-0.173027913924886,0.0462932377413482,
-0.353066666666667));
#26423=CARTESIAN_POINT('Ctrl Pts',(-0.172329203404992,0.0505785162845987,
-0.353066666666667));
#26424=CARTESIAN_POINT('Ctrl Pts',(-0.171466216089777,0.0548440796465449,
-0.353066666666667));
#26425=CARTESIAN_POINT('Ctrl Pts',(-0.170443770858798,0.0590830450887544,
-0.353066666666667));
#26426=CARTESIAN_POINT('Ctrl Pts',(-0.169609721657169,0.0625409376346687,
-0.353066666666667));
#26427=CARTESIAN_POINT('Ctrl Pts',(-0.168670590048696,0.0659761408646361,
-0.353066666666667));
#26428=CARTESIAN_POINT('Ctrl Pts',(-0.167632215380544,0.0693775142202088,
-0.353066666666667));
#26429=CARTESIAN_POINT('Ctrl Pts',(-0.164320261147807,0.0802263852757378,
-0.353066666666667));
#26430=CARTESIAN_POINT('Ctrl Pts',(-0.159996262524131,0.0907540317964261,
-0.353066666666667));
#26431=CARTESIAN_POINT('Ctrl Pts',(-0.154765649419082,0.100842798226835,
-0.353066666666667));
#26432=CARTESIAN_POINT('Ctrl Pts',(-0.151244749192667,0.107633883572982,
-0.353066666666667));
#26433=CARTESIAN_POINT('Ctrl Pts',(-0.147312170821561,0.114226277258753,
-0.353066666666667));
#26434=CARTESIAN_POINT('Ctrl Pts',(-0.142990633106768,0.120582557101035,
-0.353066666666667));
#26435=CARTESIAN_POINT('Ctrl Pts',(-0.140763809064083,0.123857853467507,
-0.353066666666667));
#26436=CARTESIAN_POINT('Ctrl Pts',(-0.138432060381342,0.127072002597403,
-0.353066666666667));
#26437=CARTESIAN_POINT('Ctrl Pts',(-0.136009717220075,0.130205302389434,
-0.353066666666667));
#26438=CARTESIAN_POINT('Ctrl Pts',(-0.128162696792256,0.140355419791331,
-0.353066666666667));
#26439=CARTESIAN_POINT('Ctrl Pts',(-0.119348186315525,0.149691156683439,
-0.353066666666667));
#26440=CARTESIAN_POINT('Ctrl Pts',(-0.109686793021438,0.158050862960414,
-0.353066666666667));
#26441=CARTESIAN_POINT('Ctrl Pts',(-0.102323091479692,0.164422447278171,
-0.353066666666667));
#26442=CARTESIAN_POINT('Ctrl Pts',(-0.0944662156361962,0.170227170930749,
-0.353066666666667));
#26443=CARTESIAN_POINT('Ctrl Pts',(-0.0861525859670518,0.175382131162755,
-0.353066666666667));
#26444=CARTESIAN_POINT('Ctrl Pts',(-0.0905442217324539,-0.126745838915641,
-0.353066666666667));
#26445=CARTESIAN_POINT('Ctrl Pts',(-0.0531162262373072,-0.153109051305698,
-0.349777237901969));
#26446=CARTESIAN_POINT('Ctrl Pts',(0.0522750989337435,-0.172567827516364,
-0.342834954190459));
#26447=CARTESIAN_POINT('Ctrl Pts',(0.173623780493455,-0.0578082499262578,
-0.332239815532139));
#26448=CARTESIAN_POINT('Ctrl Pts',(0.144299756757966,0.112561276791376,
-0.321281250691706));
#26449=CARTESIAN_POINT('Ctrl Pts',(-0.0137605119892857,0.182468951639323,
-0.310322685851272));
#26450=CARTESIAN_POINT('Ctrl Pts',(-0.136232288784936,0.104481976189832,
-0.301115950322802));
#26451=CARTESIAN_POINT('Ctrl Pts',(-0.155286340637538,0.0266232940100586,
-0.295562069741144));
#26452=CARTESIAN_POINT('Ctrl Pts',(-0.15531185862521,-1.5337286706104E-5,
-0.293661044106296));
#26453=CARTESIAN_POINT('Origin',(-2.59090492670967E-17,0.,-0.353066666666667));
#26454=CARTESIAN_POINT('',(-0.1954,-2.39295984553393E-17,-0.353066666666667));
#26455=CARTESIAN_POINT('Origin',(0.,0.,-0.353066666666667));
#26456=CARTESIAN_POINT('Origin',(0.,0.,-0.353066666666667));
#26457=CARTESIAN_POINT('',(0.090360677865019,-0.126612599672285,-0.353066666666667));
#26458=CARTESIAN_POINT('Ctrl Pts',(0.0863529496556134,0.175584683415656,
-0.353066666666667));
#26459=CARTESIAN_POINT('Ctrl Pts',(0.091775925641401,0.172264613803354,
-0.353066666666667));
#26460=CARTESIAN_POINT('Ctrl Pts',(0.0970151064363841,0.168672722682513,
-0.353066666666667));
#26461=CARTESIAN_POINT('Ctrl Pts',(0.102046076702462,0.164808456407418,
-0.353066666666667));
#26462=CARTESIAN_POINT('Ctrl Pts',(0.109748329747439,0.158892389503854,
-0.353066666666667));
#26463=CARTESIAN_POINT('Ctrl Pts',(0.11696333598913,0.152338121455057,-0.353066666666667));
#26464=CARTESIAN_POINT('Ctrl Pts',(0.123648657619329,0.145228304456469,
-0.353066666666667));
#26465=CARTESIAN_POINT('Ctrl Pts',(0.126392710732544,0.14231001322853,-0.353066666666667));
#26466=CARTESIAN_POINT('Ctrl Pts',(0.129045803306702,0.139299406002297,
-0.353066666666667));
#26467=CARTESIAN_POINT('Ctrl Pts',(0.131599361332803,0.136209297313463,
-0.353066666666667));
#26468=CARTESIAN_POINT('Ctrl Pts',(0.136248057252147,0.130583822777432,
-0.353066666666667));
#26469=CARTESIAN_POINT('Ctrl Pts',(0.140573104671842,0.124688829108862,
-0.353066666666667));
#26470=CARTESIAN_POINT('Ctrl Pts',(0.144556667852106,0.118560041485065,
-0.353066666666667));
#26471=CARTESIAN_POINT('Ctrl Pts',(0.147882589890062,0.113443047251125,
-0.353066666666667));
#26472=CARTESIAN_POINT('Ctrl Pts',(0.150970393632736,0.108162994083143,
-0.353066666666667));
#26473=CARTESIAN_POINT('Ctrl Pts',(0.153806693424657,0.102740045379718,
-0.353066666666667));
#26474=CARTESIAN_POINT('Ctrl Pts',(0.155695835469646,0.0991280434211665,
-0.353066666666667));
#26475=CARTESIAN_POINT('Ctrl Pts',(0.157468792252594,0.0954612486662374,
-0.353066666666667));
#26476=CARTESIAN_POINT('Ctrl Pts',(0.159121858455566,0.0917483027491353,
-0.353066666666667));
#26477=CARTESIAN_POINT('Ctrl Pts',(0.164086071592859,0.0805982018840912,
-0.353066666666667));
#26478=CARTESIAN_POINT('Ctrl Pts',(0.167976354467203,0.0690254035666524,
-0.353066666666667));
#26479=CARTESIAN_POINT('Ctrl Pts',(0.170691731659898,0.0571968233482779,
-0.353066666666667));
#26480=CARTESIAN_POINT('Ctrl Pts',(0.171976315344167,0.0516009889288562,
-0.353066666666667));
#26481=CARTESIAN_POINT('Ctrl Pts',(0.172997217266348,0.0459478680695661,
-0.353066666666667));
#26482=CARTESIAN_POINT('Ctrl Pts',(0.173739546526888,0.0402557306321508,
-0.353066666666667));
#26483=CARTESIAN_POINT('Ctrl Pts',(0.174228988637866,0.0365027170956556,
-0.353066666666667));
#26484=CARTESIAN_POINT('Ctrl Pts',(0.174597145890101,0.0327307795264523,
-0.353066666666667));
#26485=CARTESIAN_POINT('Ctrl Pts',(0.174838710766854,0.0289627049718209,
-0.353066666666667));
#26486=CARTESIAN_POINT('Ctrl Pts',(0.175337568406377,0.0211812228162318,
-0.353066666666667));
#26487=CARTESIAN_POINT('Ctrl Pts',(0.175299889017541,0.0134005598576949,
-0.353066666666667));
#26488=CARTESIAN_POINT('Ctrl Pts',(0.174695429084084,0.00566655864109738,
-0.353066666666667));
#26489=CARTESIAN_POINT('Ctrl Pts',(0.1741598428623,-0.00118621068504322,
-0.353066666666667));
#26490=CARTESIAN_POINT('Ctrl Pts',(0.173179021113242,-0.00800243245789652,
-0.353066666666667));
#26491=CARTESIAN_POINT('Ctrl Pts',(0.171772005196112,-0.0147481282838624,
-0.353066666666667));
#26492=CARTESIAN_POINT('Ctrl Pts',(0.170726249047483,-0.0197618262818046,
-0.353066666666667));
#26493=CARTESIAN_POINT('Ctrl Pts',(0.169444930850078,-0.0247365274644173,
-0.353066666666667));
#26494=CARTESIAN_POINT('Ctrl Pts',(0.167934206696833,-0.0296569328335628,
-0.353066666666667));
#26495=CARTESIAN_POINT('Ctrl Pts',(0.166832256855383,-0.0332459665461353,
-0.353066666666667));
#26496=CARTESIAN_POINT('Ctrl Pts',(0.165610219623287,-0.0367990811940273,
-0.353066666666667));
#26497=CARTESIAN_POINT('Ctrl Pts',(0.164274304450244,-0.0403041213275535,
-0.353066666666667));
#26498=CARTESIAN_POINT('Ctrl Pts',(0.160829473997209,-0.0493423216824256,
-0.353066666666667));
#26499=CARTESIAN_POINT('Ctrl Pts',(0.156624378199029,-0.0580767247737816,
-0.353066666666667));
#26500=CARTESIAN_POINT('Ctrl Pts',(0.151713593210745,-0.0664101273423615,
-0.353066666666667));
#26501=CARTESIAN_POINT('Ctrl Pts',(0.148533489359529,-0.0718066343499594,
-0.353066666666667));
#26502=CARTESIAN_POINT('Ctrl Pts',(0.145056996731404,-0.0770347033166309,
-0.353066666666667));
#26503=CARTESIAN_POINT('Ctrl Pts',(0.141295320169661,-0.082063260429383,
-0.353066666666667));
#26504=CARTESIAN_POINT('Ctrl Pts',(0.138558394341238,-0.0857219449589262,
-0.353066666666667));
#26505=CARTESIAN_POINT('Ctrl Pts',(0.135667276928843,-0.0892779006893289,
-0.353066666666667));
#26506=CARTESIAN_POINT('Ctrl Pts',(0.13264496147214,-0.0926975714274839,
-0.353066666666667));
#26507=CARTESIAN_POINT('Ctrl Pts',(0.125506731853708,-0.100774291180298,
-0.353066666666667));
#26508=CARTESIAN_POINT('Ctrl Pts',(0.117622588801953,-0.108117960820719,
-0.353066666666667));
#26509=CARTESIAN_POINT('Ctrl Pts',(0.109058683323211,-0.1145742204159,-0.353066666666667));
#26510=CARTESIAN_POINT('Ctrl Pts',(0.103144935763732,-0.119032547229425,
-0.353066666666667));
#26511=CARTESIAN_POINT('Ctrl Pts',(0.0969064199016059,-0.123066975878573,
-0.353066666666667));
#26512=CARTESIAN_POINT('Ctrl Pts',(0.0903606778650195,-0.126612599672284,
-0.353066666666667));
#26513=CARTESIAN_POINT('Origin',(0.,0.,-0.353066666666667));
#26514=CARTESIAN_POINT('Origin',(0.,0.,-0.482472289227037));
#26515=CARTESIAN_POINT('Ctrl Pts',(0.090360677865019,-0.126612599672285,
-0.353066666666667));
#26516=CARTESIAN_POINT('Ctrl Pts',(0.131874352891076,-0.0969851863995775,
-0.349413811719856));
#26517=CARTESIAN_POINT('Ctrl Pts',(0.182857874798175,0.00573779165809946,
-0.342108101826233));
#26518=CARTESIAN_POINT('Ctrl Pts',(0.0963663073753999,0.155697320567796,
-0.3311495369858));
#26519=CARTESIAN_POINT('Ctrl Pts',(-0.0761582306436912,0.166338694028791,
-0.320190972145365));
#26520=CARTESIAN_POINT('Ctrl Pts',(-0.151457270014338,0.0672989293663021,
-0.312298556225779));
#26521=CARTESIAN_POINT('Ctrl Pts',(-0.155721140989265,0.00830051131805939,
-0.308058995253002));
#26522=CARTESIAN_POINT('Ctrl Pts',(-0.155653088469525,0.000125523659554115,
-0.307472289227037));
#26523=CARTESIAN_POINT('Ctrl Pts',(0.113509973994373,-0.159049193030951,
-0.376074074893873));
#26524=CARTESIAN_POINT('Ctrl Pts',(0.165658942815277,-0.121831600273079,
-0.372421219947062));
#26525=CARTESIAN_POINT('Ctrl Pts',(0.229703817007801,0.00720774342650353,
-0.365115510053439));
#26526=CARTESIAN_POINT('Ctrl Pts',(0.121054172042129,0.195585062288314,
-0.354156945213007));
#26527=CARTESIAN_POINT('Ctrl Pts',(-0.0956690341869317,0.208952624964486,
-0.343198380372572));
#26528=CARTESIAN_POINT('Ctrl Pts',(-0.22700621729006,0.0362066800668334,
-0.332239815532139));
#26529=CARTESIAN_POINT('Ctrl Pts',(-0.15587805676934,-0.168977471396189,
-0.321281250691706));
#26530=CARTESIAN_POINT('Ctrl Pts',(0.0543075797275565,-0.223358798671181,
-0.310322685851272));
#26531=CARTESIAN_POINT('Ctrl Pts',(0.216043556493043,-0.0785414608874288,
-0.299364121010839));
#26532=CARTESIAN_POINT('Ctrl Pts',(0.185071090564807,0.136355543216117,
-0.288405556170405));
#26533=CARTESIAN_POINT('Ctrl Pts',(-0.0109877667305077,0.229612032449797,
-0.277446991329971));
#26534=CARTESIAN_POINT('Ctrl Pts',(-0.197244472898579,0.118058803257178,
-0.266488426489538));
#26535=CARTESIAN_POINT('Ctrl Pts',(-0.207558494710389,-0.0988064563337987,
-0.255529861649104));
#26536=CARTESIAN_POINT('Ctrl Pts',(-0.0327288714983575,-0.227534271296709,
-0.244571296808671));
#26537=CARTESIAN_POINT('Ctrl Pts',(0.171294954925333,-0.153300998465301,
-0.233612731968237));
#26538=CARTESIAN_POINT('Ctrl Pts',(0.222522760696156,0.0576780642727636,
-0.222654167127804));
#26539=CARTESIAN_POINT('Ctrl Pts',(0.0752589587035167,0.217207742637096,
-0.21169560228737));
#26540=CARTESIAN_POINT('Ctrl Pts',(-0.139136279132604,0.182986979233611,
-0.200737037446937));
#26541=CARTESIAN_POINT('Ctrl Pts',(-0.229421104700159,-0.0144592892217846,
-0.189778472606503));
#26542=CARTESIAN_POINT('Ctrl Pts',(-0.115061091986856,-0.19900774667556,
-0.178819907766069));
#26543=CARTESIAN_POINT('Ctrl Pts',(0.101934294664377,-0.206040183664755,
-0.167861342925636));
#26544=CARTESIAN_POINT('Ctrl Pts',(0.228003284630101,-0.0292835421690294,
-0.156902778085202));
#26545=CARTESIAN_POINT('Ctrl Pts',(0.150692832428747,0.173594109330608,
-0.145944213244769));
#26546=CARTESIAN_POINT('Ctrl Pts',(-0.0610380283237141,0.221624958463411,
-0.134985648404335));
#26547=CARTESIAN_POINT('Ctrl Pts',(-0.21831968438096,0.0719647960828687,
-0.124027083563902));
#26548=CARTESIAN_POINT('Ctrl Pts',(-0.180864527330742,-0.14188786234924,
-0.113068518723468));
#26549=CARTESIAN_POINT('Ctrl Pts',(0.0179335408659357,-0.229176716732969,
-0.102109953883035));
#26550=CARTESIAN_POINT('Ctrl Pts',(0.200714315904756,-0.112036733041374,
-0.0911513890426012));
#26551=CARTESIAN_POINT('Ctrl Pts',(0.204495895156562,0.105037056726432,
-0.0801928242021676));
#26552=CARTESIAN_POINT('Ctrl Pts',(0.0257911334986473,0.228424087614811,
-0.0692342593617342));
#26553=CARTESIAN_POINT('Ctrl Pts',(-0.175776163519519,0.148042236946653,
-0.0582756945213006));
#26554=CARTESIAN_POINT('Ctrl Pts',(-0.220826613807624,-0.0643679717979928,
-0.047317129680867));
#26555=CARTESIAN_POINT('Ctrl Pts',(-0.0683468568897243,-0.219418554973255,
-0.0363585648404335));
#26556=CARTESIAN_POINT('Ctrl Pts',(0.0731165658398347,-0.192197273548725,
-0.0290528549468112));
#26557=CARTESIAN_POINT('Ctrl Pts',(0.122919639333555,-0.151894444487311,
-0.0254));
#26558=CARTESIAN_POINT('Ctrl Pts',(0.105793541951255,-0.148236995244729,
-0.368404938818138));
#26559=CARTESIAN_POINT('Ctrl Pts',(0.154397412840543,-0.113549462315245,
-0.364752083871327));
#26560=CARTESIAN_POINT('Ctrl Pts',(0.214088502937926,0.0067177595037024,
-0.357446373977704));
#26561=CARTESIAN_POINT('Ctrl Pts',(0.112824883819886,0.182289148381474,
-0.346487809137271));
#26562=CARTESIAN_POINT('Ctrl Pts',(-0.0891654330058515,0.194747981319255,
-0.335529244296837));
#26563=CARTESIAN_POINT('Ctrl Pts',(-0.211574286619625,0.033745342297022,
-0.324570679456403));
#26564=CARTESIAN_POINT('Ctrl Pts',(-0.145281433496979,-0.15749034714655,
-0.313612114615971));
#26565=CARTESIAN_POINT('Ctrl Pts',(0.0506157389698917,-0.208174820290003,
-0.302653549775536));
#26566=CARTESIAN_POINT('Ctrl Pts',(0.201356869822541,-0.0732021957622769,
-0.291694984935103));
#26567=CARTESIAN_POINT('Ctrl Pts',(0.172489918679772,0.127086064544738,
-0.280736420094669));
#26568=CARTESIAN_POINT('Ctrl Pts',(-0.0102408160239047,0.21400295791359,
-0.269777855254236));
#26569=CARTESIAN_POINT('Ctrl Pts',(-0.183835751907435,0.110033140838552,
-0.258819290413802));
#26570=CARTESIAN_POINT('Ctrl Pts',(-0.193448624334734,-0.0920895725315098,
-0.247860725573369));
#26571=CARTESIAN_POINT('Ctrl Pts',(-0.0305039558906986,-0.212066443403201,
-0.236902160732935));
#26572=CARTESIAN_POINT('Ctrl Pts',(0.159650287655161,-0.142879564161578,
-0.225943595892502));
#26573=CARTESIAN_POINT('Ctrl Pts',(0.207395616353369,0.0537570972627508,
-0.214985031052068));
#26574=CARTESIAN_POINT('Ctrl Pts',(0.0701428387711811,0.202441914346259,
-0.204026466211635));
#26575=CARTESIAN_POINT('Ctrl Pts',(-0.129677765445408,0.170547485677727,
-0.193067901371201));
#26576=CARTESIAN_POINT('Ctrl Pts',(-0.21382500947276,-0.0134763436818869,
-0.182109336530767));
#26577=CARTESIAN_POINT('Ctrl Pts',(-0.107239214614499,-0.185479157960068,
-0.171150771690334));
#26578=CARTESIAN_POINT('Ctrl Pts',(0.095004779750738,-0.192033528395153,
-0.1601922068499));
#26579=CARTESIAN_POINT('Ctrl Pts',(0.212503573110978,-0.0272928407779753,
-0.149233642009467));
#26580=CARTESIAN_POINT('Ctrl Pts',(0.1404487018039,0.161793145057621,-0.138275077169034));
#26581=CARTESIAN_POINT('Ctrl Pts',(-0.056888650246778,0.20655884690632,
-0.1273165123286));
#26582=CARTESIAN_POINT('Ctrl Pts',(-0.203478266055164,0.067072614022305,
-0.116357947488167));
#26583=CARTESIAN_POINT('Ctrl Pts',(-0.168569318504181,-0.132242295452929,
-0.105399382647733));
#26584=CARTESIAN_POINT('Ctrl Pts',(0.0167144149643532,-0.213597235051276,
-0.0944408178072993));
#26585=CARTESIAN_POINT('Ctrl Pts',(0.18706971425207,-0.104420452229878,
-0.0834822529668657));
#26586=CARTESIAN_POINT('Ctrl Pts',(0.190594220946413,0.0978966153914813,
-0.0725236881264321));
#26587=CARTESIAN_POINT('Ctrl Pts',(0.0240378467877621,0.212895769819775,
-0.0615651232859986));
#26588=CARTESIAN_POINT('Ctrl Pts',(-0.163826862741196,0.137978294363364,
-0.0506065584455651));
#26589=CARTESIAN_POINT('Ctrl Pts',(-0.205814773889109,-0.0599922234592858,
-0.0396479936051315));
#26590=CARTESIAN_POINT('Ctrl Pts',(-0.0637006231008205,-0.204502435192149,
-0.028689428764698));
#26591=CARTESIAN_POINT('Ctrl Pts',(0.0681460862275567,-0.179131662237028,
-0.0213837188710756));
#26592=CARTESIAN_POINT('Ctrl Pts',(0.114563536250235,-0.141568628020543,
-0.0177308639242644));
#26593=CARTESIAN_POINT('Ctrl Pts',(0.098077109908137,-0.137424797458507,
-0.360735802742402));
#26594=CARTESIAN_POINT('Ctrl Pts',(0.14313588286581,-0.105267324357411,
-0.357082947795591));
#26595=CARTESIAN_POINT('Ctrl Pts',(0.19847318886805,0.0062277755809008,
-0.349777237901968));
#26596=CARTESIAN_POINT('Ctrl Pts',(0.104595595597643,0.168993234474635,
-0.338818673061536));
#26597=CARTESIAN_POINT('Ctrl Pts',(-0.0826618318247713,0.180543337674023,
-0.327860108221101));
#26598=CARTESIAN_POINT('Ctrl Pts',(-0.19614235594919,0.031284004527211,
-0.316901543380668));
#26599=CARTESIAN_POINT('Ctrl Pts',(-0.134684810224618,-0.146003222896912,
-0.305942978540235));
#26600=CARTESIAN_POINT('Ctrl Pts',(0.0469238982122269,-0.192990841908825,
-0.294984413699801));
#26601=CARTESIAN_POINT('Ctrl Pts',(0.18667018315204,-0.0678629306371251,
-0.284025848859368));
#26602=CARTESIAN_POINT('Ctrl Pts',(0.159908746794737,0.117816585873359,
-0.273067284018934));
#26603=CARTESIAN_POINT('Ctrl Pts',(-0.00949386531730154,0.198393883377383,
-0.2621087191785));
#26604=CARTESIAN_POINT('Ctrl Pts',(-0.170427030916291,0.102007478419926,
-0.251150154338067));
#26605=CARTESIAN_POINT('Ctrl Pts',(-0.179338753959079,-0.0853726887292205,
-0.240191589497633));
#26606=CARTESIAN_POINT('Ctrl Pts',(-0.0282790402830398,-0.196598615509695,
-0.2292330246572));
#26607=CARTESIAN_POINT('Ctrl Pts',(0.14800562038499,-0.132458129857856,
-0.218274459816766));
#26608=CARTESIAN_POINT('Ctrl Pts',(0.192268472010582,0.0498361302527376,
-0.207315894976333));
#26609=CARTESIAN_POINT('Ctrl Pts',(0.0650267188388455,0.187676086055423,
-0.196357330135899));
#26610=CARTESIAN_POINT('Ctrl Pts',(-0.120219251758212,0.158107992121843,
-0.185398765295466));
#26611=CARTESIAN_POINT('Ctrl Pts',(-0.198228914245361,-0.0124933981419889,
-0.174440200455032));
#26612=CARTESIAN_POINT('Ctrl Pts',(-0.0994173372421406,-0.171950569244577,
-0.163481635614598));
#26613=CARTESIAN_POINT('Ctrl Pts',(0.0880752648370985,-0.178026873125552,
-0.152523070774165));
#26614=CARTESIAN_POINT('Ctrl Pts',(0.197003861591856,-0.0253021393869213,
-0.141564505933731));
#26615=CARTESIAN_POINT('Ctrl Pts',(0.130204571179052,0.149992180784635,
-0.130605941093298));
#26616=CARTESIAN_POINT('Ctrl Pts',(-0.0527392721698415,0.191492735349228,
-0.119647376252864));
#26617=CARTESIAN_POINT('Ctrl Pts',(-0.188636847729369,0.0621804319617416,
-0.108688811412431));
#26618=CARTESIAN_POINT('Ctrl Pts',(-0.15627410967762,-0.122596728556619,
-0.097730246571997));
#26619=CARTESIAN_POINT('Ctrl Pts',(0.015495289062771,-0.198017753369582,
-0.0867716817315639));
#26620=CARTESIAN_POINT('Ctrl Pts',(0.173425112599384,-0.0968041714183824,
-0.07581311689113));
#26621=CARTESIAN_POINT('Ctrl Pts',(0.176692546736265,0.0907561740565302,
-0.0648545520506967));
#26622=CARTESIAN_POINT('Ctrl Pts',(0.0222845600768763,0.197367452024739,
-0.053895987210263));
#26623=CARTESIAN_POINT('Ctrl Pts',(-0.151877561962873,0.127914351780075,
-0.0429374223698296));
#26624=CARTESIAN_POINT('Ctrl Pts',(-0.190802933970593,-0.0556164751205788,
-0.031978857529396));
#26625=CARTESIAN_POINT('Ctrl Pts',(-0.0590543893119163,-0.189586315411043,
-0.0210202926889625));
#26626=CARTESIAN_POINT('Ctrl Pts',(0.0631756066152784,-0.166066050925332,
-0.0137145827953401));
#26627=CARTESIAN_POINT('Ctrl Pts',(0.106207433166915,-0.131242811553775,
-0.0100617278485289));
#26628=CARTESIAN_POINT('Ctrl Pts',(0.090360677865019,-0.126612599672285,
-0.353066666666667));
#26629=CARTESIAN_POINT('Ctrl Pts',(0.131874352891076,-0.0969851863995775,
-0.349413811719856));
#26630=CARTESIAN_POINT('Ctrl Pts',(0.182857874798175,0.00573779165809946,
-0.342108101826233));
#26631=CARTESIAN_POINT('Ctrl Pts',(0.0963663073753999,0.155697320567796,
-0.3311495369858));
#26632=CARTESIAN_POINT('Ctrl Pts',(-0.0761582306436912,0.166338694028791,
-0.320190972145365));
#26633=CARTESIAN_POINT('Ctrl Pts',(-0.180710425278755,0.0288226667573998,
-0.309232407304933));
#26634=CARTESIAN_POINT('Ctrl Pts',(-0.124088186952256,-0.134516098647273,
-0.298273842464499));
#26635=CARTESIAN_POINT('Ctrl Pts',(0.0432320574545622,-0.177806863527647,
-0.287315277624065));
#26636=CARTESIAN_POINT('Ctrl Pts',(0.171983496481539,-0.0625236655119731,
-0.276356712783632));
#26637=CARTESIAN_POINT('Ctrl Pts',(0.147327574909702,0.10854710720198,-0.265398147943198));
#26638=CARTESIAN_POINT('Ctrl Pts',(-0.00874691461069841,0.182784808841176,
-0.254439583102765));
#26639=CARTESIAN_POINT('Ctrl Pts',(-0.157018309925148,0.0939818160013004,
-0.243481018262331));
#26640=CARTESIAN_POINT('Ctrl Pts',(-0.165228883583424,-0.0786558049269315,
-0.232522453421898));
#26641=CARTESIAN_POINT('Ctrl Pts',(-0.0260541246753813,-0.181130787616187,
-0.221563888581464));
#26642=CARTESIAN_POINT('Ctrl Pts',(0.136360953114818,-0.122036695554133,
-0.21060532374103));
#26643=CARTESIAN_POINT('Ctrl Pts',(0.177141327667794,0.0459151632427247,
-0.199646758900597));
#26644=CARTESIAN_POINT('Ctrl Pts',(0.0599105989065099,0.172910257764587,
-0.188688194060163));
#26645=CARTESIAN_POINT('Ctrl Pts',(-0.110760738071016,0.145668498565958,
-0.17772962921973));
#26646=CARTESIAN_POINT('Ctrl Pts',(-0.182632819017962,-0.0115104526020911,
-0.166771064379296));
#26647=CARTESIAN_POINT('Ctrl Pts',(-0.0915954598697826,-0.158421980529086,
-0.155812499538863));
#26648=CARTESIAN_POINT('Ctrl Pts',(0.081145749923459,-0.16402021785595,
-0.144853934698429));
#26649=CARTESIAN_POINT('Ctrl Pts',(0.181504150072734,-0.0233114379958674,
-0.133895369857996));
#26650=CARTESIAN_POINT('Ctrl Pts',(0.119960440554205,0.138191216511648,
-0.122936805017562));
#26651=CARTESIAN_POINT('Ctrl Pts',(-0.0485898940929054,0.176426623792137,
-0.111978240177129));
#26652=CARTESIAN_POINT('Ctrl Pts',(-0.173795429403574,0.057288249901178,
-0.101019675336695));
#26653=CARTESIAN_POINT('Ctrl Pts',(-0.143978900851059,-0.112951161660308,
-0.0900611104962616));
#26654=CARTESIAN_POINT('Ctrl Pts',(0.0142761631611888,-0.182438271687888,
-0.0791025456558283));
#26655=CARTESIAN_POINT('Ctrl Pts',(0.159780510946698,-0.0891878906068867,
-0.0681439808153946));
#26656=CARTESIAN_POINT('Ctrl Pts',(0.162790872526117,0.083615732721579,
-0.0571854159749611));
#26657=CARTESIAN_POINT('Ctrl Pts',(0.0205312733659909,0.181839134229702,
-0.0462268511345275));
#26658=CARTESIAN_POINT('Ctrl Pts',(-0.13992826118455,0.117850409196786,
-0.035268286294094));
#26659=CARTESIAN_POINT('Ctrl Pts',(-0.175791094052078,-0.051240726781872,
-0.0243097214536604));
#26660=CARTESIAN_POINT('Ctrl Pts',(-0.0544081555230124,-0.174670195629937,
-0.0133511566132269));
#26661=CARTESIAN_POINT('Ctrl Pts',(0.0582051270030004,-0.153000439613635,
-0.00604544671960458));
#26662=CARTESIAN_POINT('Ctrl Pts',(0.0978513300835948,-0.120916995087007,
-0.00239259177279338));
#26663=CARTESIAN_POINT('Ctrl Pts',(0.122919639333553,-0.151894444487312,
-0.0254000000000001));
#26664=CARTESIAN_POINT('Ctrl Pts',(0.0731165658398337,-0.192197273548725,
-0.0290528549468112));
#26665=CARTESIAN_POINT('Ctrl Pts',(0.00238485447505431,-0.20580791426099,
-0.0327057098936224));
#26666=CARTESIAN_POINT('Ctrl Pts',(-0.058394294026985,-0.186771470754579,
-0.0363585648404336));
#26667=CARTESIAN_POINT('Ctrl Pts',(-0.119173442529025,-0.167735027248167,
-0.0400114197872447));
#26668=CARTESIAN_POINT('Ctrl Pts',(-0.170000028168324,-0.11605149952308,
-0.0436642747340559));
#26669=CARTESIAN_POINT('Ctrl Pts',(-0.187904912606623,-0.0548080342030955,
-0.0473171296808671));
#26670=CARTESIAN_POINT('Ctrl Pts',(-0.193072141284385,-0.0371335838922075,
-0.0483713189386592));
#26671=CARTESIAN_POINT('Ctrl Pts',(-0.195497451170818,-0.0186629240423492,
-0.0494255081964514));
#26672=CARTESIAN_POINT('Ctrl Pts',(-0.195345140381879,-0.000154736422984442,
-0.0504796974542436));
#26673=CARTESIAN_POINT('Origin',(0.,0.,-0.199));
#26674=CARTESIAN_POINT('',(0.0577350269189626,-0.1,-0.199));
#26675=CARTESIAN_POINT('',(-0.0577350269189627,-0.1,-0.199));
#26676=CARTESIAN_POINT('',(0.0288675134594813,-0.1,-0.199));
#26677=CARTESIAN_POINT('Origin',(0.,0.,-0.199));
#26678=CARTESIAN_POINT('Origin',(0.,0.,-0.199));
#26679=CARTESIAN_POINT('',(-0.115470053837925,2.77555756156289E-17,-0.199));
#26680=CARTESIAN_POINT('',(-0.0721687836487033,-0.075,-0.199));
#26681=CARTESIAN_POINT('Origin',(0.,0.,-0.199));
#26682=CARTESIAN_POINT('Origin',(0.,0.,-0.199));
#26683=CARTESIAN_POINT('',(-0.0577350269189626,0.1,-0.199));
#26684=CARTESIAN_POINT('',(-0.101036297108185,0.025,-0.199));
#26685=CARTESIAN_POINT('Origin',(0.,0.,-0.199));
#26686=CARTESIAN_POINT('Origin',(0.,0.,-0.199));
#26687=CARTESIAN_POINT('',(0.0577350269189626,0.1,-0.199));
#26688=CARTESIAN_POINT('',(-0.0288675134594813,0.1,-0.199));
#26689=CARTESIAN_POINT('Origin',(0.,0.,-0.199));
#26690=CARTESIAN_POINT('Origin',(0.,0.,-0.199));
#26691=CARTESIAN_POINT('',(0.115470053837925,0.,-0.199));
#26692=CARTESIAN_POINT('',(0.0721687836487032,0.075,-0.199));
#26693=CARTESIAN_POINT('Origin',(0.,0.,-0.199));
#26694=CARTESIAN_POINT('Origin',(0.,0.,-0.199));
#26695=CARTESIAN_POINT('',(0.101036297108185,-0.025,-0.199));
#26696=CARTESIAN_POINT('Origin',(0.,0.,-0.199));
#26697=CARTESIAN_POINT('Origin',(0.,0.,-0.234141016151378));
#26698=CARTESIAN_POINT('',(0.,0.,-0.269282032302755));
#26699=CARTESIAN_POINT('',(-0.113827101150665,-1.39397995080384E-17,-0.2));
#26700=CARTESIAN_POINT('',(-0.0577350269189626,-7.07050159149938E-18,-0.234141016151378));
#26701=CARTESIAN_POINT('',(-0.113789894775128,-0.00291012086156119,-0.2));
#26702=CARTESIAN_POINT('Origin',(0.,0.,-0.2));
#26703=CARTESIAN_POINT('Ctrl Pts',(-0.115470053837925,-1.38777878078145E-17,
-0.199));
#26704=CARTESIAN_POINT('Ctrl Pts',(-0.114623954995367,-0.00146548618353618,
-0.199514986736453));
#26705=CARTESIAN_POINT('Ctrl Pts',(-0.113789894775128,-0.00291012086156124,
-0.2));
#26706=CARTESIAN_POINT('',(-0.0594151859817593,-0.0970898791384388,-0.2));
#26707=CARTESIAN_POINT('Ctrl Pts',(-0.0594151859817594,-0.0970898791384387,
-0.2));
#26708=CARTESIAN_POINT('Ctrl Pts',(-0.0585811257615208,-0.0985345138164641,
-0.199514986736453));
#26709=CARTESIAN_POINT('Ctrl Pts',(-0.0577350269189627,-0.1,-0.199));
#26710=CARTESIAN_POINT('',(-0.0543747087933692,-0.1,-0.2));
#26711=CARTESIAN_POINT('Origin',(0.,0.,-0.2));
#26712=CARTESIAN_POINT('Ctrl Pts',(-0.0577350269189627,-0.1,-0.199));
#26713=CARTESIAN_POINT('Ctrl Pts',(-0.0560428292338519,-0.1,-0.199514986736451));
#26714=CARTESIAN_POINT('Ctrl Pts',(-0.0543747087933692,-0.1,-0.2));
#26715=CARTESIAN_POINT('',(0.0543747087933691,-0.1,-0.2));
#26716=CARTESIAN_POINT('Ctrl Pts',(0.0543747087933691,-0.1,-0.2));
#26717=CARTESIAN_POINT('Ctrl Pts',(0.056042829233854,-0.1,-0.19951498673645));
#26718=CARTESIAN_POINT('Ctrl Pts',(0.0577350269189626,-0.1,-0.199));
#26719=CARTESIAN_POINT('',(0.0594151859817594,-0.0970898791384387,-0.2));
#26720=CARTESIAN_POINT('Origin',(0.,0.,-0.2));
#26721=CARTESIAN_POINT('Ctrl Pts',(0.0577350269189626,-0.1,-0.199));
#26722=CARTESIAN_POINT('Ctrl Pts',(0.0585811257615188,-0.0985345138164674,
-0.199514986736451));
#26723=CARTESIAN_POINT('Ctrl Pts',(0.0594151859817594,-0.0970898791384387,
-0.2));
#26724=CARTESIAN_POINT('',(0.113789894775128,-0.00291012086156127,-0.2));
#26725=CARTESIAN_POINT('Ctrl Pts',(0.113789894775128,-0.00291012086156127,
-0.2));
#26726=CARTESIAN_POINT('Ctrl Pts',(0.114623954995369,-0.00146548618353307,
-0.199514986736452));
#26727=CARTESIAN_POINT('Ctrl Pts',(0.115470053837925,1.38777878078145E-17,
-0.199));
#26728=CARTESIAN_POINT('',(0.113789894775128,0.00291012086156127,-0.2));
#26729=CARTESIAN_POINT('Origin',(0.,0.,-0.2));
#26730=CARTESIAN_POINT('Ctrl Pts',(0.115470053837925,0.,-0.199));
#26731=CARTESIAN_POINT('Ctrl Pts',(0.114623954995369,0.00146548618353293,
-0.199514986736452));
#26732=CARTESIAN_POINT('Ctrl Pts',(0.113789894775128,0.00291012086156128,
-0.2));
#26733=CARTESIAN_POINT('',(0.0594151859817593,0.0970898791384387,-0.2));
#26734=CARTESIAN_POINT('Ctrl Pts',(0.0594151859817593,0.0970898791384387,
-0.2));
#26735=CARTESIAN_POINT('Ctrl Pts',(0.0585811257615177,0.0985345138164694,
-0.199514986736451));
#26736=CARTESIAN_POINT('Ctrl Pts',(0.0577350269189626,0.1,-0.199));
#26737=CARTESIAN_POINT('',(0.0543747087933691,0.1,-0.2));
#26738=CARTESIAN_POINT('Origin',(0.,0.,-0.2));
#26739=CARTESIAN_POINT('Ctrl Pts',(0.0577350269189626,0.1,-0.199));
#26740=CARTESIAN_POINT('Ctrl Pts',(0.0560428292338471,0.1,-0.199514986736452));
#26741=CARTESIAN_POINT('Ctrl Pts',(0.0543747087933691,0.1,-0.2));
#26742=CARTESIAN_POINT('',(-0.0543747087933691,0.1,-0.2));
#26743=CARTESIAN_POINT('Ctrl Pts',(-0.0543747087933691,0.1,-0.2));
#26744=CARTESIAN_POINT('Ctrl Pts',(-0.0560428292338464,0.1,-0.199514986736453));
#26745=CARTESIAN_POINT('Ctrl Pts',(-0.0577350269189626,0.1,-0.199));
#26746=CARTESIAN_POINT('',(-0.0594151859817593,0.0970898791384387,-0.2));
#26747=CARTESIAN_POINT('Origin',(0.,0.,-0.2));
#26748=CARTESIAN_POINT('Ctrl Pts',(-0.0577350269189626,0.1,-0.199));
#26749=CARTESIAN_POINT('Ctrl Pts',(-0.0585811257615179,0.0985345138164689,
-0.199514986736451));
#26750=CARTESIAN_POINT('Ctrl Pts',(-0.0594151859817593,0.0970898791384388,
-0.2));
#26751=CARTESIAN_POINT('',(-0.113789894775128,0.0029101208615613,-0.2));
#26752=CARTESIAN_POINT('Ctrl Pts',(-0.113789894775128,0.00291012086156131,
-0.2));
#26753=CARTESIAN_POINT('Ctrl Pts',(-0.11462395499537,0.00146548618353128,
-0.199514986736451));
#26754=CARTESIAN_POINT('Ctrl Pts',(-0.115470053837925,2.08166817117217E-17,
-0.199));
#26755=CARTESIAN_POINT('Origin',(0.,0.,-0.2));
#26756=CARTESIAN_POINT('Origin',(-0.115470053837925,1.38777878078145E-17,
0.));
#26757=CARTESIAN_POINT('',(-0.0577350269189626,0.1,0.));
#26758=CARTESIAN_POINT('',(-0.0577350269189626,0.1,0.));
#26759=CARTESIAN_POINT('',(-0.115470053837925,1.41410031829988E-17,0.));
#26760=CARTESIAN_POINT('',(-0.101036297108185,0.025,0.));
#26761=CARTESIAN_POINT('',(-0.115470053837925,1.41410031829988E-17,0.));
#26762=CARTESIAN_POINT('Origin',(-0.115470053837925,1.38777878078145E-17,
0.));
#26763=CARTESIAN_POINT('',(-0.115470053837925,1.38777878078145E-17,-0.2));
#26764=CARTESIAN_POINT('',(-0.115470053837925,1.41410031829988E-17,0.));
#26765=CARTESIAN_POINT('',(-0.0577350269189626,0.1,-0.2));
#26766=CARTESIAN_POINT('Origin',(-0.0577350269189626,0.1,0.));
#26767=CARTESIAN_POINT('',(0.0577350269189626,0.1,0.));
#26768=CARTESIAN_POINT('',(0.0577350269189626,0.1,0.));
#26769=CARTESIAN_POINT('',(-0.0288675134594813,0.1,0.));
#26770=CARTESIAN_POINT('Origin',(-0.0577350269189626,0.1,0.));
#26771=CARTESIAN_POINT('',(0.0577350269189626,0.1,-0.2));
#26772=CARTESIAN_POINT('',(0.0577350269189626,0.1,-0.2));
#26773=CARTESIAN_POINT('',(0.0577350269189626,0.1,0.));
#26774=CARTESIAN_POINT('Origin',(-0.0577350269189626,0.1,0.));
#26775=CARTESIAN_POINT('',(-0.0577350269189626,0.1,-0.2));
#26776=CARTESIAN_POINT('',(-0.0577350269189626,0.1,0.));
#26777=CARTESIAN_POINT('',(0.0577350269189626,0.1,-0.2));
#26778=CARTESIAN_POINT('Origin',(-0.0577350269189626,-0.1,0.));
#26779=CARTESIAN_POINT('',(-0.0577350269189626,-0.1,0.));
#26780=CARTESIAN_POINT('',(-0.0721687836487033,-0.075,0.));
#26781=CARTESIAN_POINT('',(-0.0577350269189626,-0.1,0.));
#26782=CARTESIAN_POINT('Origin',(-0.0577350269189626,-0.1,0.));
#26783=CARTESIAN_POINT('',(-0.0577350269189626,-0.1,-0.2));
#26784=CARTESIAN_POINT('',(-0.0577350269189626,-0.1,0.));
#26785=CARTESIAN_POINT('',(-0.115470053837925,1.41410031829988E-17,-0.2));
#26786=CARTESIAN_POINT('Origin',(0.0577350269189626,0.1,0.));
#26787=CARTESIAN_POINT('',(0.115470053837925,0.,0.));
#26788=CARTESIAN_POINT('',(0.115470053837925,0.,0.));
#26789=CARTESIAN_POINT('',(0.0721687836487032,0.075,0.));
#26790=CARTESIAN_POINT('Origin',(0.0577350269189626,0.1,0.));
#26791=CARTESIAN_POINT('',(0.115470053837925,0.,-0.2));
#26792=CARTESIAN_POINT('',(0.115470053837925,0.,-0.2));
#26793=CARTESIAN_POINT('',(0.115470053837925,0.,0.));
#26794=CARTESIAN_POINT('Origin',(0.0577350269189626,0.1,0.));
#26795=CARTESIAN_POINT('',(0.115470053837925,0.,-0.2));
#26796=CARTESIAN_POINT('Origin',(0.,0.,-0.2));
#26797=CARTESIAN_POINT('',(-0.0577350269189626,0.1,-0.2));
#26798=CARTESIAN_POINT('Origin',(0.,0.,-0.2));
#26799=CARTESIAN_POINT('Origin',(0.,0.,-0.2));
#26800=CARTESIAN_POINT('',(0.0577350269189626,-0.1,-0.2));
#26801=CARTESIAN_POINT('Origin',(0.,0.,-0.2));
#26802=CARTESIAN_POINT('',(0.0577350269189626,-0.1,-0.2));
#26803=CARTESIAN_POINT('',(-0.0577350269189626,-0.1,-0.2));
#26804=CARTESIAN_POINT('',(0.0577350269189626,-0.1,-0.2));
#26805=CARTESIAN_POINT('Origin',(0.,0.,-0.2));
#26806=CARTESIAN_POINT('',(-0.0577350269189626,-0.1,-0.2));
#26807=CARTESIAN_POINT('Origin',(0.,0.,-0.2));
#26808=CARTESIAN_POINT('',(-0.115470053837925,1.41410031829988E-17,-0.2));
#26809=CARTESIAN_POINT('Origin',(0.115470053837925,0.,0.));
#26810=CARTESIAN_POINT('',(0.0577350269189626,-0.1,0.));
#26811=CARTESIAN_POINT('',(0.0577350269189626,-0.1,0.));
#26812=CARTESIAN_POINT('',(0.101036297108185,-0.025,0.));
#26813=CARTESIAN_POINT('Origin',(0.115470053837925,0.,0.));
#26814=CARTESIAN_POINT('',(0.0577350269189626,-0.1,0.));
#26815=CARTESIAN_POINT('Origin',(0.115470053837925,0.,0.));
#26816=CARTESIAN_POINT('Origin',(0.0577350269189626,-0.1,0.));
#26817=CARTESIAN_POINT('Origin',(0.0577350269189626,-0.1,0.));
#26818=CARTESIAN_POINT('',(0.0288675134594813,-0.1,0.));
#26819=CARTESIAN_POINT('Origin',(-0.115470053837925,1.38777878078145E-17,
0.));
#26820=CARTESIAN_POINT('Origin',(-0.0577350269189626,-0.1,0.));
#26821=CARTESIAN_POINT('Origin',(0.0577350269189626,-0.1,0.));
#26822=CARTESIAN_POINT('Origin',(0.125,0.,-0.4));
#26823=CARTESIAN_POINT('',(-0.125,-1.53080849893419E-17,-0.4));
#26824=CARTESIAN_POINT('Origin',(0.,0.,-0.4));
#26825=CARTESIAN_POINT('Origin',(0.,0.,-0.375));
#26826=CARTESIAN_POINT('',(-0.1625,-1.99005104861445E-17,-0.375));
#26827=CARTESIAN_POINT('Origin',(0.,0.,-0.19));
#26828=CARTESIAN_POINT('Origin',(0.,0.,-0.0254));
#26829=CARTESIAN_POINT('Origin',(0.,0.,-0.015));
#26830=CARTESIAN_POINT('',(-0.17,-2.0818995585505E-17,-1.73472347597681E-18));
#26831=CARTESIAN_POINT('Origin',(0.,0.,0.));
#26832=CARTESIAN_POINT('',(-0.185,-2.2655965784226E-17,-0.015));
#26833=CARTESIAN_POINT('Origin',(0.,0.,0.));
#26834=CARTESIAN_POINT('',(0.,0.,0.));
#26835=CARTESIAN_POINT('Origin',(0.,-1.3456066017178,6.2893933982822));
#26836=CARTESIAN_POINT('',(-2.885,-1.3562132034356,6.285));
#26837=CARTESIAN_POINT('',(-2.8787867965644,-1.3712132034356,6.2787867965644));
#26838=CARTESIAN_POINT('',(-2.82767686307234,-1.49460349804412,6.22767686307234));
#26839=CARTESIAN_POINT('',(2.8787867965644,-1.3712132034356,6.2787867965644));
#26840=CARTESIAN_POINT('',(0.,-1.3712132034356,6.2787867965644));
#26841=CARTESIAN_POINT('',(2.885,-1.3562132034356,6.285));
#26842=CARTESIAN_POINT('',(2.82767686307234,-1.49460349804412,6.22767686307234));
#26843=CARTESIAN_POINT('',(2.87,-1.32,6.3));
#26844=CARTESIAN_POINT('',(2.489697839644,-0.401869366668709,6.68030216035601));
#26845=CARTESIAN_POINT('',(-2.87,-1.32,6.3));
#26846=CARTESIAN_POINT('',(0.,-1.32,6.3));
#26847=CARTESIAN_POINT('',(-2.489697839644,-0.401869366668709,6.68030216035601));
#26848=CARTESIAN_POINT('Origin',(2.885,2.77555756156289E-17,6.285));
#26849=CARTESIAN_POINT('',(2.9,-1.32,6.27));
#26850=CARTESIAN_POINT('',(2.97292879382193,-1.14393431686758,6.19707120617807));
#26851=CARTESIAN_POINT('',(2.9,0.1,6.27));
#26852=CARTESIAN_POINT('',(2.9,2.77555756156289E-17,6.27));
#26853=CARTESIAN_POINT('',(2.87,0.1,6.3));
#26854=CARTESIAN_POINT('',(2.87,0.1,6.3));
#26855=CARTESIAN_POINT('',(2.87,2.77555756156289E-17,6.3));
#26856=CARTESIAN_POINT('Origin',(2.8893933982822,-1.3456066017178,8.2125));
#26857=CARTESIAN_POINT('',(2.8787867965644,-1.3712132034356,5.7287867965644));
#26858=CARTESIAN_POINT('',(2.8787867965644,-1.3712132034356,8.2125));
#26859=CARTESIAN_POINT('',(2.9,-1.32,5.78));
#26860=CARTESIAN_POINT('',(2.8787867965644,-1.3712132034356,5.7287867965644));
#26861=CARTESIAN_POINT('',(2.9,-1.32,8.2125));
#26862=CARTESIAN_POINT('Origin',(0.,-1.375,6.275));
#26863=CARTESIAN_POINT('',(-2.8712132034356,-1.3787867965644,6.2712132034356));
#26864=CARTESIAN_POINT('',(-2.6125,-1.6375,6.0125));
#26865=CARTESIAN_POINT('',(2.8712132034356,-1.3787867965644,6.2712132034356));
#26866=CARTESIAN_POINT('',(0.,-1.3787867965644,6.2712132034356));
#26867=CARTESIAN_POINT('',(2.6125,-1.6375,6.0125));
#26868=CARTESIAN_POINT('Origin',(0.,-1.3456066017178,5.7106066017178));
#26869=CARTESIAN_POINT('',(-2.82,-1.32,5.7));
#26870=CARTESIAN_POINT('',(2.82,-1.32,5.7));
#26871=CARTESIAN_POINT('',(0.,-1.32,5.7));
#26872=CARTESIAN_POINT('',(2.8712132034356,-1.3712132034356,5.7212132034356));
#26873=CARTESIAN_POINT('',(2.82,-1.32,5.7));
#26874=CARTESIAN_POINT('',(-2.8712132034356,-1.3712132034356,5.7212132034356));
#26875=CARTESIAN_POINT('',(0.,-1.3712132034356,5.7212132034356));
#26876=CARTESIAN_POINT('',(-2.8712132034356,-1.3712132034356,5.7212132034356));
#26877=CARTESIAN_POINT('Origin',(2.8456066017178,-1.1,5.7106066017178));
#26878=CARTESIAN_POINT('',(2.82,0.95,5.7));
#26879=CARTESIAN_POINT('',(2.82,-1.1,5.7));
#26880=CARTESIAN_POINT('',(2.8712132034356,0.971213203435597,5.7212132034356));
#26881=CARTESIAN_POINT('',(1.47300280204935,0.392055492130272,5.14205549213028));
#26882=CARTESIAN_POINT('',(2.8712132034356,-1.1,5.7212132034356));
#26883=CARTESIAN_POINT('Origin',(-2.8456066017178,-1.1,5.7106066017178));
#26884=CARTESIAN_POINT('',(-2.8712132034356,0.971213203435597,5.7212132034356));
#26885=CARTESIAN_POINT('',(-2.8712132034356,-1.1,5.7212132034356));
#26886=CARTESIAN_POINT('',(-2.82,0.95,5.7));
#26887=CARTESIAN_POINT('',(-1.47300280204935,0.392055492130272,5.14205549213028));
#26888=CARTESIAN_POINT('',(-2.82,-1.1,5.7));
#26889=CARTESIAN_POINT('Origin',(0.,-1.4,5.7));
#26890=CARTESIAN_POINT('',(-0.733143914930758,0.950000000000001,5.7));
#26891=CARTESIAN_POINT('',(0.,0.95,5.7));
#26892=CARTESIAN_POINT('',(-1.2,1.46957615897682E-16,5.7));
#26893=CARTESIAN_POINT('Origin',(0.,0.,5.7));
#26894=CARTESIAN_POINT('',(0.733143914930758,0.950000000000001,5.7));
#26895=CARTESIAN_POINT('Origin',(0.,0.,5.7));
#26896=CARTESIAN_POINT('',(0.,0.95,5.7));
#26897=CARTESIAN_POINT('Ctrl Pts',(0.234492626320026,1.17686584120771,5.2));
#26898=CARTESIAN_POINT('Ctrl Pts',(0.234492626320026,1.17686584120771,5.21851592037048));
#26899=CARTESIAN_POINT('Ctrl Pts',(0.230065594000457,1.17776475629821,5.25703220095455));
#26900=CARTESIAN_POINT('Ctrl Pts',(0.208561308949327,1.18184858998349,5.31286098873592));
#26901=CARTESIAN_POINT('Ctrl Pts',(0.175078618630889,1.18735985109294,5.35981780168936));
#26902=CARTESIAN_POINT('Ctrl Pts',(0.132977608595357,1.19291479882069,5.39638849063154));
#26903=CARTESIAN_POINT('Ctrl Pts',(0.0797919333124946,1.19779759041496,
5.42375237476982));
#26904=CARTESIAN_POINT('Ctrl Pts',(0.0270809220838994,1.20001767329007,
5.43500694450787));
#26905=CARTESIAN_POINT('Ctrl Pts',(-0.0286029864222697,1.20010475087302,
5.43548184690207));
#26906=CARTESIAN_POINT('Ctrl Pts',(-0.0673004953048968,1.19832870594691,
5.42640311279717));
#26907=CARTESIAN_POINT('Ctrl Pts',(-0.118808426842686,1.19445759764994,
5.40509087371658));
#26908=CARTESIAN_POINT('Ctrl Pts',(-0.145105499862307,1.19138154283581,
5.38703853259485));
#26909=CARTESIAN_POINT('Ctrl Pts',(-0.186607973526257,1.18557851967241,
5.34540463031795));
#26910=CARTESIAN_POINT('Ctrl Pts',(-0.204599918973935,1.18248717481483,
5.31905282963216));
#26911=CARTESIAN_POINT('Ctrl Pts',(-0.228496361591337,1.17808596546445,
5.26111603578263));
#26912=CARTESIAN_POINT('Ctrl Pts',(-0.234425323120645,1.17685953455129,
5.22956894464554));
#26913=CARTESIAN_POINT('Ctrl Pts',(-0.234294478758728,1.17688759738335,
5.17767894605582));
#26914=CARTESIAN_POINT('Ctrl Pts',(-0.228111094333853,1.17818452128479,
5.13119983678783));
#26915=CARTESIAN_POINT('Ctrl Pts',(-0.196601450552936,1.18397925051513,
5.06597720676137));
#26916=CARTESIAN_POINT('Ctrl Pts',(-0.152167749680949,1.19070622188097,
5.01676689334197));
#26917=CARTESIAN_POINT('Ctrl Pts',(-0.0915400219194833,1.19713526569684,
4.97952753552852));
#26918=CARTESIAN_POINT('Ctrl Pts',(-0.0222401922789184,1.20045910805244,
4.96273883536335));
#26919=CARTESIAN_POINT('Ctrl Pts',(0.0335828950866025,1.19987839029729,
4.96556047978417));
#26920=CARTESIAN_POINT('Ctrl Pts',(0.102259384899266,1.19636361322958,4.98396469296537));
#26921=CARTESIAN_POINT('Ctrl Pts',(0.142497929826391,1.19174220944178,5.01030250445097));
#26922=CARTESIAN_POINT('Ctrl Pts',(0.186690885906675,1.18557585757076,5.05453934674594));
#26923=CARTESIAN_POINT('Ctrl Pts',(0.204662083875366,1.18248576762501,5.08088946271256));
#26924=CARTESIAN_POINT('Ctrl Pts',(0.228592229859133,1.1780835276557,5.13881431659721));
#26925=CARTESIAN_POINT('Ctrl Pts',(0.234492626320026,1.17686584120771,5.17037400265145));
#26926=CARTESIAN_POINT('Ctrl Pts',(0.234492626320026,1.17686584120771,5.2));
#26927=CARTESIAN_POINT('Ctrl Pts',(0.224661750880017,1.16869720356482,5.2));
#26928=CARTESIAN_POINT('Ctrl Pts',(0.224664044082871,1.16869658022503,5.21784968514182));
#26929=CARTESIAN_POINT('Ctrl Pts',(0.220347781825578,1.16953151025151,5.25499826456546));
#26930=CARTESIAN_POINT('Ctrl Pts',(0.199462940996693,1.17331171992303,5.30869422291513));
#26931=CARTESIAN_POINT('Ctrl Pts',(0.167106453640583,1.17839956757166,5.35364934929127));
#26932=CARTESIAN_POINT('Ctrl Pts',(0.126660674993384,1.1835094683978,5.38846950726549));
#26933=CARTESIAN_POINT('Ctrl Pts',(0.0758545072020466,1.18798593044828,
5.41438801389221));
#26934=CARTESIAN_POINT('Ctrl Pts',(0.0257341972508752,1.19001518718189,
5.42499940578561));
#26935=CARTESIAN_POINT('Ctrl Pts',(-0.0271662575703232,1.19009521901816,
5.4254491044883));
#26936=CARTESIAN_POINT('Ctrl Pts',(-0.0639694888884449,1.18847148693327,
5.41688611040433));
#26937=CARTESIAN_POINT('Ctrl Pts',(-0.113097318603888,1.18492738150962,
5.39672394786756));
#26938=CARTESIAN_POINT('Ctrl Pts',(-0.138291037166866,1.1821013903319,5.37958710544409));
#26939=CARTESIAN_POINT('Ctrl Pts',(-0.178227153593058,1.17675766202459,
5.33986702046425));
#26940=CARTESIAN_POINT('Ctrl Pts',(-0.195628209030011,1.17390150521058,
5.31462522547444));
#26941=CARTESIAN_POINT('Ctrl Pts',(-0.218819386947306,1.16982933241391,
5.25892872162705));
#26942=CARTESIAN_POINT('Ctrl Pts',(-0.224587941395262,1.1686929086115,5.2285063395467));
#26943=CARTESIAN_POINT('Ctrl Pts',(-0.224471866771419,1.1687172800089,5.17847879299728));
#26944=CARTESIAN_POINT('Ctrl Pts',(-0.218433291914077,1.16992270346931,
5.13365077066068));
#26945=CARTESIAN_POINT('Ctrl Pts',(-0.187868345911638,1.17528340489058,
5.07099553678837));
#26946=CARTESIAN_POINT('Ctrl Pts',(-0.145053403930571,1.18148068253972,
5.02402161588194));
#26947=CARTESIAN_POINT('Ctrl Pts',(-0.0870347413400359,1.18738127001952,
4.98869879876734));
#26948=CARTESIAN_POINT('Ctrl Pts',(-0.0211261762958701,1.19041889729488,
4.97287241139659));
#26949=CARTESIAN_POINT('Ctrl Pts',(0.0318967819082349,1.18988874316386,
4.97552771036542));
#26950=CARTESIAN_POINT('Ctrl Pts',(0.0972569740091445,1.18667356122128,
4.9929056676729));
#26951=CARTESIAN_POINT('Ctrl Pts',(0.135784681753249,1.18243415718769,5.01787150746554));
#26952=CARTESIAN_POINT('Ctrl Pts',(0.178307565473129,1.17675446720244,5.06007864635613));
#26953=CARTESIAN_POINT('Ctrl Pts',(0.195692635440334,1.1739004547617,5.08531514197247));
#26954=CARTESIAN_POINT('Ctrl Pts',(0.218912554144602,1.16982655564952,5.14100422188478));
#26955=CARTESIAN_POINT('Ctrl Pts',(0.224660105409413,1.16869963356623,5.17143164799448));
#26956=CARTESIAN_POINT('Ctrl Pts',(0.224661750880017,1.16869720356482,5.2));
#26957=CARTESIAN_POINT('Ctrl Pts',(0.214830875440008,1.16052856592193,5.2));
#26958=CARTESIAN_POINT('Ctrl Pts',(0.214828582237154,1.16052918926171,5.21719693319092));
#26959=CARTESIAN_POINT('Ctrl Pts',(0.210634710406464,1.16129601125582,5.25295676722098));
#26960=CARTESIAN_POINT('Ctrl Pts',(0.190362570396196,1.16477491560071,5.30453079295661));
#26961=CARTESIAN_POINT('Ctrl Pts',(0.159134503245928,1.16944043352991,5.34748758598507));
#26962=CARTESIAN_POINT('Ctrl Pts',(0.120331596908531,1.17410858214668,5.38057170621492));
#26963=CARTESIAN_POINT('Ctrl Pts',(0.0719132086075718,1.17817752530137,
5.40503842533525));
#26964=CARTESIAN_POINT('Ctrl Pts',(0.0243663461721618,1.18001467471676,
5.4150055273476));
#26965=CARTESIAN_POINT('Ctrl Pts',(-0.0257415711068092,1.18008692449041,
5.41542929395432));
#26966=CARTESIAN_POINT('Ctrl Pts',(-0.0606502732383226,1.1786161400379,
5.40738216145846));
#26967=CARTESIAN_POINT('Ctrl Pts',(-0.107389914733047,1.17539276698966,
5.38835446764134));
#26968=CARTESIAN_POINT('Ctrl Pts',(-0.131489864383231,1.17282131064298,
5.3721457714085));
#26969=CARTESIAN_POINT('Ctrl Pts',(-0.169849523031342,1.16793341659147,
5.33433090190193));
#26970=CARTESIAN_POINT('Ctrl Pts',(-0.186680035883757,1.16531442344864,
5.31021018521442));
#26971=CARTESIAN_POINT('Ctrl Pts',(-0.209144973553841,1.16157006705547,
5.2567474710098));
#26972=CARTESIAN_POINT('Ctrl Pts',(-0.214785043930596,1.16052068738504,
5.22746776581041));
#26973=CARTESIAN_POINT('Ctrl Pts',(-0.214649541396742,1.16054630709438,
5.17927946000339));
#26974=CARTESIAN_POINT('Ctrl Pts',(-0.208777651148686,1.16165383773602,
5.13611567681124));
#26975=CARTESIAN_POINT('Ctrl Pts',(-0.179153953237642,1.16658250125997,
5.0760273252867));
#26976=CARTESIAN_POINT('Ctrl Pts',(-0.137910376824399,1.17226130085929,
5.03125163794571));
#26977=CARTESIAN_POINT('Ctrl Pts',(-0.0825171178287952,1.17762891532049,
4.99786508496316));
#26978=CARTESIAN_POINT('Ctrl Pts',(-0.0199848479662072,1.18038001208676,
4.98300022887185));
#26979=CARTESIAN_POINT('Ctrl Pts',(0.0302169894530887,1.17989998331047,
4.98549037212516));
#26980=CARTESIAN_POINT('Ctrl Pts',(0.0922643071693305,1.17698583602376,
5.00183735778633));
#26981=CARTESIAN_POINT('Ctrl Pts',(0.129073305025927,1.17312581435099,5.02543896237632));
#26982=CARTESIAN_POINT('Ctrl Pts',(0.169922090789214,1.167932896833,5.06561751781489));
#26983=CARTESIAN_POINT('Ctrl Pts',(0.186728468423531,1.16531399806998,5.08974201762226));
#26984=CARTESIAN_POINT('Ctrl Pts',(0.209226990165204,1.16156954658368,5.14319234394881));
#26985=CARTESIAN_POINT('Ctrl Pts',(0.214832520910613,1.16052613592052,5.17249276942433));
#26986=CARTESIAN_POINT('Ctrl Pts',(0.214830875440008,1.16052856592193,5.2));
#26987=CARTESIAN_POINT('Ctrl Pts',(0.204999999999999,1.15235992827903,5.2));
#26988=CARTESIAN_POINT('Ctrl Pts',(0.204999999999999,1.15235992827903,5.21653069796226));
#26989=CARTESIAN_POINT('Ctrl Pts',(0.200916898231585,1.15306276520912,5.25092283083188));
#26990=CARTESIAN_POINT('Ctrl Pts',(0.181264202443562,1.15623804554025,5.30036402713581));
#26991=CARTESIAN_POINT('Ctrl Pts',(0.151162338255622,1.16048015000863,5.34131913358699));
#26992=CARTESIAN_POINT('Ctrl Pts',(0.114014663306557,1.16470325172378,5.37265272284888));
#26993=CARTESIAN_POINT('Ctrl Pts',(0.0679757824971238,1.16836586533469,
5.39567406445764));
#26994=CARTESIAN_POINT('Ctrl Pts',(0.0230196213391375,1.17001218860859,
5.40499798862534));
#26995=CARTESIAN_POINT('Ctrl Pts',(-0.0243048422548627,1.17007739263555,
5.40539655154055));
#26996=CARTESIAN_POINT('Ctrl Pts',(-0.0573192668218707,1.16875892102426,
5.39786515906562));
#26997=CARTESIAN_POINT('Ctrl Pts',(-0.101678806494249,1.16586255084935,
5.37998754179231));
#26998=CARTESIAN_POINT('Ctrl Pts',(-0.124675401687789,1.16354115813907,
5.36469434425773));
#26999=CARTESIAN_POINT('Ctrl Pts',(-0.161468703098142,1.15911255894365,
5.32879329204822));
#27000=CARTESIAN_POINT('Ctrl Pts',(-0.177708325939833,1.15672875384439,
5.30578258105671));
#27001=CARTESIAN_POINT('Ctrl Pts',(-0.19946799890981,1.15331343400492,5.25456015685422));
#27002=CARTESIAN_POINT('Ctrl Pts',(-0.204947662205213,1.15235406144525,
5.22640516071157));
#27003=CARTESIAN_POINT('Ctrl Pts',(-0.204826929409432,1.15237598971992,
5.18007930694485));
#27004=CARTESIAN_POINT('Ctrl Pts',(-0.19909984872891,1.15339201992053,5.13856661068409));
#27005=CARTESIAN_POINT('Ctrl Pts',(-0.170420848596344,1.15788665563542,
5.08104565531369));
#27006=CARTESIAN_POINT('Ctrl Pts',(-0.130796031074021,1.16303576151804,
5.03850636048567));
#27007=CARTESIAN_POINT('Ctrl Pts',(-0.0780118372493478,1.16787491964318,
5.00703634820198));
#27008=CARTESIAN_POINT('Ctrl Pts',(-0.0188708319831588,1.1703398013292,
4.99313380490508));
#27009=CARTESIAN_POINT('Ctrl Pts',(0.0285308762747211,1.16991033617703,
4.99545760270642));
#27010=CARTESIAN_POINT('Ctrl Pts',(0.0872618962792086,1.16729578401546,
5.01077833249387));
#27011=CARTESIAN_POINT('Ctrl Pts',(0.122360056952786,1.16381776209691,5.03300796539089));
#27012=CARTESIAN_POINT('Ctrl Pts',(0.161538770355668,1.15911150646468,5.07115681742508));
#27013=CARTESIAN_POINT('Ctrl Pts',(0.177759019988499,1.15672868520667,5.09416769688216));
#27014=CARTESIAN_POINT('Ctrl Pts',(0.199547314450672,1.1533125745775,5.14538224923639));
#27015=CARTESIAN_POINT('Ctrl Pts',(0.204999999999999,1.15235992827903,5.17355041476736));
#27016=CARTESIAN_POINT('Ctrl Pts',(0.204999999999999,1.15235992827903,5.2));
#27017=CARTESIAN_POINT('',(0.234492626320026,1.17686584120771,5.2));
#27018=CARTESIAN_POINT('',(0.204999999999999,1.15235992827903,5.2));
#27019=CARTESIAN_POINT('',(0.234492626320026,1.17686584120771,5.2));
#27020=CARTESIAN_POINT('',(-4.97473164011138E-6,1.17000356538632,4.99499072157072));
#27021=CARTESIAN_POINT('Ctrl Pts',(0.204999999999999,1.15235992827903,5.2));
#27022=CARTESIAN_POINT('Ctrl Pts',(0.204999999999999,1.15235992827903,5.21653069796226));
#27023=CARTESIAN_POINT('Ctrl Pts',(0.200916898231585,1.15306276520912,5.25092283083188));
#27024=CARTESIAN_POINT('Ctrl Pts',(0.181264202443562,1.15623804554025,5.30036402713581));
#27025=CARTESIAN_POINT('Ctrl Pts',(0.151162338255622,1.16048015000863,5.34131913358699));
#27026=CARTESIAN_POINT('Ctrl Pts',(0.114014663306557,1.16470325172378,5.37265272284888));
#27027=CARTESIAN_POINT('Ctrl Pts',(0.0679757824971238,1.16836586533469,
5.39567406445764));
#27028=CARTESIAN_POINT('Ctrl Pts',(0.0230196213391375,1.17001218860859,
5.40499798862534));
#27029=CARTESIAN_POINT('Ctrl Pts',(-0.0243048422548627,1.17007739263555,
5.40539655154055));
#27030=CARTESIAN_POINT('Ctrl Pts',(-0.0573192668218707,1.16875892102426,
5.39786515906562));
#27031=CARTESIAN_POINT('Ctrl Pts',(-0.101678806494249,1.16586255084935,
5.37998754179231));
#27032=CARTESIAN_POINT('Ctrl Pts',(-0.124675401687789,1.16354115813907,
5.36469434425773));
#27033=CARTESIAN_POINT('Ctrl Pts',(-0.161468703098142,1.15911255894365,
5.32879329204822));
#27034=CARTESIAN_POINT('Ctrl Pts',(-0.177708325939833,1.15672875384439,
5.30578258105671));
#27035=CARTESIAN_POINT('Ctrl Pts',(-0.19946799890981,1.15331343400492,5.25456015685422));
#27036=CARTESIAN_POINT('Ctrl Pts',(-0.204947662205213,1.15235406144525,
5.22640516071157));
#27037=CARTESIAN_POINT('Ctrl Pts',(-0.204826929409432,1.15237598971992,
5.18007930694485));
#27038=CARTESIAN_POINT('Ctrl Pts',(-0.19909984872891,1.15339201992053,5.13856661068409));
#27039=CARTESIAN_POINT('Ctrl Pts',(-0.170420848596344,1.15788665563542,
5.08104565531369));
#27040=CARTESIAN_POINT('Ctrl Pts',(-0.130796031074021,1.16303576151804,
5.03850636048567));
#27041=CARTESIAN_POINT('Ctrl Pts',(-0.0780118372493478,1.16787491964318,
5.00703634820198));
#27042=CARTESIAN_POINT('Ctrl Pts',(-0.032012760281176,1.16979207140417,
4.99622313736308));
#27043=CARTESIAN_POINT('Ctrl Pts',(-0.00639669818699399,1.17000452714276,
4.99498981359792));
#27044=CARTESIAN_POINT('Ctrl Pts',(-4.97473164011615E-6,1.17000356538632,
4.99499072157072));
#27045=CARTESIAN_POINT('Ctrl Pts',(-4.97473164011615E-6,1.17000356538632,
4.99499072157072));
#27046=CARTESIAN_POINT('Ctrl Pts',(0.0127769627408511,1.17000164210058,
4.9949925373019));
#27047=CARTESIAN_POINT('Ctrl Pts',(0.0350570588945874,1.16961980751136,
4.99716004002923));
#27048=CARTESIAN_POINT('Ctrl Pts',(0.0872618962792086,1.16729578401546,
5.01077833249387));
#27049=CARTESIAN_POINT('Ctrl Pts',(0.122360056952786,1.16381776209691,5.03300796539089));
#27050=CARTESIAN_POINT('Ctrl Pts',(0.161538770355668,1.15911150646468,5.07115681742508));
#27051=CARTESIAN_POINT('Ctrl Pts',(0.177759019988499,1.15672868520667,5.09416769688216));
#27052=CARTESIAN_POINT('Ctrl Pts',(0.199547314450672,1.1533125745775,5.14538224923639));
#27053=CARTESIAN_POINT('Ctrl Pts',(0.204999999999999,1.15235992827903,5.17355041476736));
#27054=CARTESIAN_POINT('Ctrl Pts',(0.204999999999999,1.15235992827903,5.2));
#27055=CARTESIAN_POINT('Ctrl Pts',(0.234492626320026,1.17686584120771,5.2));
#27056=CARTESIAN_POINT('Ctrl Pts',(0.234492626320026,1.17686584120771,5.17037400265145));
#27057=CARTESIAN_POINT('Ctrl Pts',(0.228592229859133,1.1780835276557,5.13881431659721));
#27058=CARTESIAN_POINT('Ctrl Pts',(0.204662083875366,1.18248576762501,5.08088946271256));
#27059=CARTESIAN_POINT('Ctrl Pts',(0.186690885906675,1.18557585757076,5.05453934674594));
#27060=CARTESIAN_POINT('Ctrl Pts',(0.142497929826391,1.19174220944178,5.01030250445097));
#27061=CARTESIAN_POINT('Ctrl Pts',(0.102259384899266,1.19636361322958,4.98396469296537));
#27062=CARTESIAN_POINT('Ctrl Pts',(0.0335828950866025,1.19987839029729,
4.96556047978417));
#27063=CARTESIAN_POINT('Ctrl Pts',(-0.0222401922789184,1.20045910805244,
4.96273883536335));
#27064=CARTESIAN_POINT('Ctrl Pts',(-0.0915400219194833,1.19713526569684,
4.97952753552852));
#27065=CARTESIAN_POINT('Ctrl Pts',(-0.152167749680949,1.19070622188097,
5.01676689334197));
#27066=CARTESIAN_POINT('Ctrl Pts',(-0.196601450552936,1.18397925051513,
5.06597720676137));
#27067=CARTESIAN_POINT('Ctrl Pts',(-0.228111094333853,1.17818452128479,
5.13119983678783));
#27068=CARTESIAN_POINT('Ctrl Pts',(-0.234294478758728,1.17688759738335,
5.17767894605582));
#27069=CARTESIAN_POINT('Ctrl Pts',(-0.234425323120645,1.17685953455129,
5.22956894464554));
#27070=CARTESIAN_POINT('Ctrl Pts',(-0.228496361591337,1.17808596546445,
5.26111603578263));
#27071=CARTESIAN_POINT('Ctrl Pts',(-0.204599918973935,1.18248717481483,
5.31905282963216));
#27072=CARTESIAN_POINT('Ctrl Pts',(-0.186607973526257,1.18557851967241,
5.34540463031795));
#27073=CARTESIAN_POINT('Ctrl Pts',(-0.145105499862307,1.19138154283581,
5.38703853259485));
#27074=CARTESIAN_POINT('Ctrl Pts',(-0.118808426842686,1.19445759764994,
5.40509087371658));
#27075=CARTESIAN_POINT('Ctrl Pts',(-0.0673004953048968,1.19832870594691,
5.42640311279717));
#27076=CARTESIAN_POINT('Ctrl Pts',(-0.0286029864222697,1.20010475087302,
5.43548184690207));
#27077=CARTESIAN_POINT('Ctrl Pts',(0.0270809220838994,1.20001767329007,
5.43500694450787));
#27078=CARTESIAN_POINT('Ctrl Pts',(0.0797919333124946,1.19779759041496,
5.42375237476982));
#27079=CARTESIAN_POINT('Ctrl Pts',(0.132977608595357,1.19291479882069,5.39638849063154));
#27080=CARTESIAN_POINT('Ctrl Pts',(0.175078618630889,1.18735985109294,5.35981780168936));
#27081=CARTESIAN_POINT('Ctrl Pts',(0.208561308949327,1.18184858998349,5.31286098873592));
#27082=CARTESIAN_POINT('Ctrl Pts',(0.230065594000457,1.17776475629821,5.25703220095455));
#27083=CARTESIAN_POINT('Ctrl Pts',(0.234492626320026,1.17686584120771,5.21851592037048));
#27084=CARTESIAN_POINT('Ctrl Pts',(0.234492626320026,1.17686584120771,5.2));
#27085=CARTESIAN_POINT('Origin',(0.,0.,5.7));
#27086=CARTESIAN_POINT('',(-1.2,1.46957615897682E-16,4.78));
#27087=CARTESIAN_POINT('Origin',(0.,0.,4.78));
#27088=CARTESIAN_POINT('',(-1.2,1.46957615897682E-16,5.7));
#27089=CARTESIAN_POINT('',(-0.770454411370329,0.92,5.67));
#27090=CARTESIAN_POINT('Origin',(0.,0.,4.75000000000001));
#27091=CARTESIAN_POINT('',(0.770454411370329,0.92,5.67));
#27092=CARTESIAN_POINT('Origin',(0.,0.,5.67));
#27093=CARTESIAN_POINT('Origin',(0.,0.,4.75000000000001));
#27094=CARTESIAN_POINT('Origin',(0.,0.95,5.2));
#27095=CARTESIAN_POINT('',(0.052199831018601,0.728126483839824,5.39824272405723));
#27096=CARTESIAN_POINT('',(4.49108658880295E-5,0.73001022386789,4.99496886927581));
#27097=CARTESIAN_POINT('Ctrl Pts',(0.052199831018601,0.728126483839824,
5.39824272405723));
#27098=CARTESIAN_POINT('Ctrl Pts',(0.0982302293711315,0.724809534278522,
5.38612233463488));
#27099=CARTESIAN_POINT('Ctrl Pts',(0.138345638847835,0.717149230706244,
5.35791819673363));
#27100=CARTESIAN_POINT('Ctrl Pts',(0.179663146502877,0.70696778967891,5.30171478600323));
#27101=CARTESIAN_POINT('Ctrl Pts',(0.190478690331408,0.703787523302871,
5.27956401023439));
#27102=CARTESIAN_POINT('Ctrl Pts',(0.200029921602327,0.700875879246346,
5.24612373179211));
#27103=CARTESIAN_POINT('Ctrl Pts',(0.202134771215936,0.700214283582941,
5.23577968142387));
#27104=CARTESIAN_POINT('Ctrl Pts',(0.207647089542785,0.698446891625313,
5.19157712891713));
#27105=CARTESIAN_POINT('Ctrl Pts',(0.203489755447152,0.699929714878053,
5.15701245250423));
#27106=CARTESIAN_POINT('Ctrl Pts',(0.180823445480298,0.70658166075718,5.09972093035022));
#27107=CARTESIAN_POINT('Ctrl Pts',(0.165889838070269,0.710634834844429,
5.07678258040992));
#27108=CARTESIAN_POINT('Ctrl Pts',(0.133222196340668,0.717699405062405,
5.04269842669383));
#27109=CARTESIAN_POINT('Ctrl Pts',(0.0959130924875414,0.724650186751937,
5.0140371229421));
#27110=CARTESIAN_POINT('Ctrl Pts',(0.0407143958653069,0.729423560490129,
4.9970978585716));
#27111=CARTESIAN_POINT('Ctrl Pts',(0.0087683139836932,0.730010101818503,
4.99497497756199));
#27112=CARTESIAN_POINT('Ctrl Pts',(4.4910865888031E-5,0.73001022386789,
4.99496886927581));
#27113=CARTESIAN_POINT('Ctrl Pts',(4.4910865888031E-5,0.73001022386789,
4.99496886927581));
#27114=CARTESIAN_POINT('Ctrl Pts',(-0.0144150329885519,0.730010426177385,
4.99495874415903));
#27115=CARTESIAN_POINT('Ctrl Pts',(-0.0519814055633027,0.728864770713442,
4.99904025375886));
#27116=CARTESIAN_POINT('Ctrl Pts',(-0.100490853947505,0.723567386179355,
5.01835059987916));
#27117=CARTESIAN_POINT('Ctrl Pts',(-0.137012137156585,0.716964400696497,
5.04626166271637));
#27118=CARTESIAN_POINT('Ctrl Pts',(-0.166997619172261,0.710467577023459,
5.07729708213043));
#27119=CARTESIAN_POINT('Ctrl Pts',(-0.207199968273801,0.699117939531869,
5.14702206281837));
#27120=CARTESIAN_POINT('Ctrl Pts',(-0.209088681335109,0.698093356717381,
5.21440963098396));
#27121=CARTESIAN_POINT('Ctrl Pts',(-0.188472856825575,0.704386618397043,
5.28674848041702));
#27122=CARTESIAN_POINT('Ctrl Pts',(-0.172527170805406,0.709084583389726,
5.31545761418984));
#27123=CARTESIAN_POINT('Ctrl Pts',(-0.126074871673654,0.719302690250943,
5.3654558850147));
#27124=CARTESIAN_POINT('Ctrl Pts',(-0.0624049065864234,0.730148572765185,
5.40608102393392));
#27125=CARTESIAN_POINT('Ctrl Pts',(0.0162020118434573,0.730720485951348,
5.40772140776134));
#27126=CARTESIAN_POINT('Ctrl Pts',(0.052199831018601,0.728126483839824,
5.39824272405723));
#27127=CARTESIAN_POINT('',(-2.51052593825206E-17,0.95,4.995));
#27128=CARTESIAN_POINT('Origin',(0.,0.,5.685));
#27129=CARTESIAN_POINT('',(-0.682934843158555,0.95,5.7));
#27130=CARTESIAN_POINT('Ctrl Pts',(-0.682934843158555,0.95,5.7));
#27131=CARTESIAN_POINT('Ctrl Pts',(-0.726694627264442,0.935903263540092,
5.68590326354009));
#27132=CARTESIAN_POINT('Ctrl Pts',(-0.770454411370329,0.92,5.67));
#27133=CARTESIAN_POINT('',(0.682934843158555,0.95,5.7));
#27134=CARTESIAN_POINT('Origin',(0.,0.,5.7));
#27135=CARTESIAN_POINT('Ctrl Pts',(0.770454411370329,0.92,5.67));
#27136=CARTESIAN_POINT('Ctrl Pts',(0.726694627264442,0.935903263540092,
5.68590326354009));
#27137=CARTESIAN_POINT('Ctrl Pts',(0.682934843158555,0.950000000000001,
5.7));
#27138=CARTESIAN_POINT('Origin',(0.,3.6089936932244E-17,4.7543933982822));
#27139=CARTESIAN_POINT('',(-1.1787867965644,0.,4.7287867965644));
#27140=CARTESIAN_POINT('Origin',(0.,7.2179873864488E-17,4.7287867965644));
#27141=CARTESIAN_POINT('',(-1.1893933982822,2.17838555677817E-16,4.7543933982822));
#27142=CARTESIAN_POINT('Origin',(0.,0.,4.725));
#27143=CARTESIAN_POINT('',(-1.1712132034356,2.86864500141304E-16,4.7212132034356));
#27144=CARTESIAN_POINT('Origin',(0.,7.1716125035326E-17,4.7212132034356));
#27145=CARTESIAN_POINT('',(-1.175,1.43895998899814E-16,4.725));
#27146=CARTESIAN_POINT('Ctrl Pts',(0.0574844932621232,0.697635673567799,
5.42785529611499));
#27147=CARTESIAN_POINT('Ctrl Pts',(0.108362285081162,0.693443393568619,
5.41500017367323));
#27148=CARTESIAN_POINT('Ctrl Pts',(0.153783173631022,0.683700872584965,
5.38492528292425));
#27149=CARTESIAN_POINT('Ctrl Pts',(0.202453501259093,0.670296320458785,
5.32107996750068));
#27150=CARTESIAN_POINT('Ctrl Pts',(0.215583701847853,0.666020452558282,
5.29529098994732));
#27151=CARTESIAN_POINT('Ctrl Pts',(0.227321703930627,0.662060184763746,
5.25551407980518));
#27152=CARTESIAN_POINT('Ctrl Pts',(0.229928314309894,0.66115513119461,5.24311976375499));
#27153=CARTESIAN_POINT('Ctrl Pts',(0.236794050807431,0.658726504222929,
5.18991348571448));
#27154=CARTESIAN_POINT('Ctrl Pts',(0.231462706037527,0.66080100427468,5.14789144672313));
#27155=CARTESIAN_POINT('Ctrl Pts',(0.203869008088291,0.669781865995222,
5.08051031045204));
#27156=CARTESIAN_POINT('Ctrl Pts',(0.18605041127256,0.675154593136393,5.05431187603876));
#27157=CARTESIAN_POINT('Ctrl Pts',(0.14822387585714,0.684346822022482,5.01626492020255));
#27158=CARTESIAN_POINT('Ctrl Pts',(0.105765749697592,0.693258892245674,
4.98506844977587));
#27159=CARTESIAN_POINT('Ctrl Pts',(0.028738398930405,0.700850964995508,
4.96254287357644));
#27160=CARTESIAN_POINT('Ctrl Pts',(-0.0475862280670742,0.699755567657756,
4.96563476101538));
#27161=CARTESIAN_POINT('Ctrl Pts',(-0.111011416912225,0.691877659824728,
4.98973284239457));
#27162=CARTESIAN_POINT('Ctrl Pts',(-0.152587648961219,0.683387533301053,
5.02024984047599));
#27163=CARTESIAN_POINT('Ctrl Pts',(-0.18727301159214,0.674952805171226,
5.054836260095));
#27164=CARTESIAN_POINT('Ctrl Pts',(-0.235690308368254,0.659782116656368,
5.13510787390001));
#27165=CARTESIAN_POINT('Ctrl Pts',(-0.238469103754452,0.658266427814801,
5.21784077794351));
#27166=CARTESIAN_POINT('Ctrl Pts',(-0.213091855455513,0.666842690298363,
5.30389851392055));
#27167=CARTESIAN_POINT('Ctrl Pts',(-0.19378027571931,0.673129747072274,
5.33701028923091));
#27168=CARTESIAN_POINT('Ctrl Pts',(-0.13987348404776,0.686445436448048,
5.39292755581025));
#27169=CARTESIAN_POINT('Ctrl Pts',(-0.0681937113019595,0.700215139205497,
5.43630057604647));
#27170=CARTESIAN_POINT('Ctrl Pts',(0.0176957967597459,0.700914223020843,
5.43790857372489));
#27171=CARTESIAN_POINT('Ctrl Pts',(0.0574844932621232,0.697635673567799,
5.42785529611499));
#27172=CARTESIAN_POINT('Ctrl Pts',(0.0557229391809491,0.707799276991807,
5.4179844387624));
#27173=CARTESIAN_POINT('Ctrl Pts',(0.105006256977315,0.703890847153119,
5.40537480552625));
#27174=CARTESIAN_POINT('Ctrl Pts',(0.148647188430249,0.694846643807852,
5.3759195474566));
#27175=CARTESIAN_POINT('Ctrl Pts',(0.194854073400739,0.682520843360022,
5.31462589198225));
#27176=CARTESIAN_POINT('Ctrl Pts',(0.207222067153112,0.678606570745627,
5.29004247566461));
#27177=CARTESIAN_POINT('Ctrl Pts',(0.218223734130959,0.674998911137377,
5.25238582952766));
#27178=CARTESIAN_POINT('Ctrl Pts',(0.220668729091904,0.674171964569765,
5.24067000158302));
#27179=CARTESIAN_POINT('Ctrl Pts',(0.227069505891163,0.671972354474063,
5.19047530531853));
#27180=CARTESIAN_POINT('Ctrl Pts',(0.222134458180962,0.673846041938921,
5.15092792931724));
#27181=CARTESIAN_POINT('Ctrl Pts',(0.196192676791318,0.682045761228669,
5.08691771703881));
#27182=CARTESIAN_POINT('Ctrl Pts',(0.179330882194175,0.686979951172563,
5.06180111704474));
#27183=CARTESIAN_POINT('Ctrl Pts',(0.143226304178282,0.695464397761381,
5.02507782820571));
#27184=CARTESIAN_POINT('Ctrl Pts',(0.102484489395487,0.703719635746295,
4.99472610142197));
#27185=CARTESIAN_POINT('Ctrl Pts',(0.027906440222761,0.710793406085462,
4.97258182217268));
#27186=CARTESIAN_POINT('Ctrl Pts',(-0.0461857534028223,0.709770528979505,
4.97563057389981));
#27187=CARTESIAN_POINT('Ctrl Pts',(-0.107504270586471,0.702440826803183,
4.99927454745295));
#27188=CARTESIAN_POINT('Ctrl Pts',(-0.147397927045243,0.694582159236071,
5.02891815925868));
#27189=CARTESIAN_POINT('Ctrl Pts',(-0.180511954268061,0.68679303751798,
5.0623245317732));
#27190=CARTESIAN_POINT('Ctrl Pts',(-0.226207394094477,0.67288956482352,
5.13907079803442));
#27191=CARTESIAN_POINT('Ctrl Pts',(-0.228599451800739,0.671585435233324,
5.21671156965555));
#27192=CARTESIAN_POINT('Ctrl Pts',(-0.204924940023387,0.679330870447946,
5.29818796269183));
#27193=CARTESIAN_POINT('Ctrl Pts',(-0.18667582898087,0.68512183856289,5.32983099864382));
#27194=CARTESIAN_POINT('Ctrl Pts',(-0.135289824847769,0.697385634364381,
5.38378497251866));
#27195=CARTESIAN_POINT('Ctrl Pts',(-0.0662562200070666,0.710198992168331,
5.42622168260221));
#27196=CARTESIAN_POINT('Ctrl Pts',(0.017198689960621,0.710837005186152,
5.42787264463697));
#27197=CARTESIAN_POINT('Ctrl Pts',(0.0557229391809491,0.707799276991807,
5.4179844387624));
#27198=CARTESIAN_POINT('Ctrl Pts',(0.053961385099775,0.717962880415815,
5.40811358140981));
#27199=CARTESIAN_POINT('Ctrl Pts',(0.101586257474979,0.714362080694022,
5.39574770278186));
#27200=CARTESIAN_POINT('Ctrl Pts',(0.143481624048608,0.706003459483357,
5.36692393220129));
#27201=CARTESIAN_POINT('Ctrl Pts',(0.187262574361231,0.694743266777672,
5.30816886152166));
#27202=CARTESIAN_POINT('Ctrl Pts',(0.198840325026149,0.691201405115526,
5.28481252451709));
#27203=CARTESIAN_POINT('Ctrl Pts',(0.209127891401994,0.687937152872715,
5.24925198206962));
#27204=CARTESIAN_POINT('Ctrl Pts',(0.211394356433926,0.687197450207785,
5.23822944359584));
#27205=CARTESIAN_POINT('Ctrl Pts',(0.217371634459052,0.685201041374179,
5.19101530931308));
#27206=CARTESIAN_POINT('Ctrl Pts',(0.212818003303718,0.686884677213813,
5.15397596991012));
#27207=CARTESIAN_POINT('Ctrl Pts',(0.18849977677727,0.694317765523733,5.09331352376346));
#27208=CARTESIAN_POINT('Ctrl Pts',(0.172609367148655,0.698809476808259,
5.06929333940394));
#27209=CARTESIAN_POINT('Ctrl Pts',(0.138219768019526,0.706581829323507,
5.03388551869067));
#27210=CARTESIAN_POINT('Ctrl Pts',(0.0991943527896464,0.714189443251316,
5.004379471296));
#27211=CARTESIAN_POINT('Ctrl Pts',(0.0270579057126555,0.720734025456457,
4.98261272409452));
#27212=CARTESIAN_POINT('Ctrl Pts',(-0.0447870233167377,0.719788394834089,
4.98562305251957));
#27213=CARTESIAN_POINT('Ctrl Pts',(-0.103998000273259,0.7130042192009,5.00880889482078));
#27214=CARTESIAN_POINT('Ctrl Pts',(-0.142201859072561,0.705769774761479,
5.03759334393367));
#27215=CARTESIAN_POINT('Ctrl Pts',(-0.173758676496339,0.698627344676705,
5.06980881045223));
#27216=CARTESIAN_POINT('Ctrl Pts',(-0.216682882547578,0.686010491364717,
5.14305913868396));
#27217=CARTESIAN_POINT('Ctrl Pts',(-0.218958333288822,0.684774349298858,
5.21553883927192));
#27218=CARTESIAN_POINT('Ctrl Pts',(-0.1966397722577,0.691898438247459,5.29245903164574));
#27219=CARTESIAN_POINT('Ctrl Pts',(-0.179631617543846,0.69709249189911,
5.32263690477693));
#27220=CARTESIAN_POINT('Ctrl Pts',(-0.130658530873645,0.708362492334609,
5.37459846830629));
#27221=CARTESIAN_POINT('Ctrl Pts',(-0.0643423978813163,0.72016471980235,
5.41615991737817));
#27222=CARTESIAN_POINT('Ctrl Pts',(0.0166991186425822,0.720797703786039,
5.41775733684927));
#27223=CARTESIAN_POINT('Ctrl Pts',(0.053961385099775,0.717962880415815,
5.40811358140981));
#27224=CARTESIAN_POINT('Ctrl Pts',(0.052199831018601,0.728126483839824,
5.39824272405723));
#27225=CARTESIAN_POINT('Ctrl Pts',(0.0982302293711315,0.724809534278522,
5.38612233463488));
#27226=CARTESIAN_POINT('Ctrl Pts',(0.138345638847835,0.717149230706244,
5.35791819673363));
#27227=CARTESIAN_POINT('Ctrl Pts',(0.179663146502877,0.70696778967891,5.30171478600323));
#27228=CARTESIAN_POINT('Ctrl Pts',(0.190478690331408,0.703787523302871,
5.27956401023439));
#27229=CARTESIAN_POINT('Ctrl Pts',(0.200029921602327,0.700875879246346,
5.24612373179211));
#27230=CARTESIAN_POINT('Ctrl Pts',(0.202134771215936,0.700214283582941,
5.23577968142387));
#27231=CARTESIAN_POINT('Ctrl Pts',(0.207647089542785,0.698446891625313,
5.19157712891713));
#27232=CARTESIAN_POINT('Ctrl Pts',(0.203489755447152,0.699929714878053,
5.15701245250423));
#27233=CARTESIAN_POINT('Ctrl Pts',(0.180823445480298,0.70658166075718,5.09972093035022));
#27234=CARTESIAN_POINT('Ctrl Pts',(0.165889838070269,0.710634834844429,
5.07678258040992));
#27235=CARTESIAN_POINT('Ctrl Pts',(0.133222196340668,0.717699405062405,
5.04269842669383));
#27236=CARTESIAN_POINT('Ctrl Pts',(0.0959130924875414,0.724650186751937,
5.0140371229421));
#27237=CARTESIAN_POINT('Ctrl Pts',(0.0262259470050115,0.730676466546411,
4.99265167269076));
#27238=CARTESIAN_POINT('Ctrl Pts',(-0.0433865486524858,0.729803356155837,
4.995618865404));
#27239=CARTESIAN_POINT('Ctrl Pts',(-0.100490853947505,0.723567386179355,
5.01835059987916));
#27240=CARTESIAN_POINT('Ctrl Pts',(-0.137012137156585,0.716964400696497,
5.04626166271637));
#27241=CARTESIAN_POINT('Ctrl Pts',(-0.166997619172261,0.710467577023459,
5.07729708213043));
#27242=CARTESIAN_POINT('Ctrl Pts',(-0.207199968273801,0.699117939531869,
5.14702206281837));
#27243=CARTESIAN_POINT('Ctrl Pts',(-0.209088681335109,0.698093356717381,
5.21440963098396));
#27244=CARTESIAN_POINT('Ctrl Pts',(-0.188472856825575,0.704386618397043,
5.28674848041702));
#27245=CARTESIAN_POINT('Ctrl Pts',(-0.172527170805406,0.709084583389726,
5.31545761418984));
#27246=CARTESIAN_POINT('Ctrl Pts',(-0.126074871673654,0.719302690250943,
5.3654558850147));
#27247=CARTESIAN_POINT('Ctrl Pts',(-0.0624049065864234,0.730148572765185,
5.40608102393392));
#27248=CARTESIAN_POINT('Ctrl Pts',(0.0162020118434573,0.730720485951348,
5.40772140776134));
#27249=CARTESIAN_POINT('Ctrl Pts',(0.052199831018601,0.728126483839824,
5.39824272405723));
#27250=CARTESIAN_POINT('',(0.0574844932621232,0.697635673567799,5.42785529611499));
#27251=CARTESIAN_POINT('',(0.0574844932621232,0.697635673567799,5.42785529611499));
#27252=CARTESIAN_POINT('',(-0.202821321852304,0.670001188175288,5.08280703661229));
#27253=CARTESIAN_POINT('Ctrl Pts',(0.0574844932621232,0.697635673567799,
5.42785529611499));
#27254=CARTESIAN_POINT('Ctrl Pts',(0.0176957967597459,0.700914223020843,
5.43790857372489));
#27255=CARTESIAN_POINT('Ctrl Pts',(-0.0681937113019595,0.700215139205497,
5.43630057604647));
#27256=CARTESIAN_POINT('Ctrl Pts',(-0.13987348404776,0.686445436448048,
5.39292755581025));
#27257=CARTESIAN_POINT('Ctrl Pts',(-0.19378027571931,0.673129747072274,
5.33701028923091));
#27258=CARTESIAN_POINT('Ctrl Pts',(-0.213091855455513,0.666842690298363,
5.30389851392055));
#27259=CARTESIAN_POINT('Ctrl Pts',(-0.238469103754452,0.658266427814801,
5.21784077794351));
#27260=CARTESIAN_POINT('Ctrl Pts',(-0.236213308908359,0.65949684697199,
5.15067913679837));
#27261=CARTESIAN_POINT('Ctrl Pts',(-0.208439846266026,0.668297710235964,
5.09269649867272));
#27262=CARTESIAN_POINT('Ctrl Pts',(-0.202821321852304,0.670001188175288,
5.08280703661229));
#27263=CARTESIAN_POINT('',(0.202776724457231,0.669982292593922,5.08288957607631));
#27264=CARTESIAN_POINT('Ctrl Pts',(-0.202821321852304,0.670001188175288,
5.08280703661229));
#27265=CARTESIAN_POINT('Ctrl Pts',(-0.195534564259789,0.672210456996427,
5.06998122907843));
#27266=CARTESIAN_POINT('Ctrl Pts',(-0.17972259321901,0.676788903208357,
5.0473073799466));
#27267=CARTESIAN_POINT('Ctrl Pts',(-0.152587648961219,0.683387533301053,
5.02024984047599));
#27268=CARTESIAN_POINT('Ctrl Pts',(-0.111011416912225,0.691877659824728,
4.98973284239457));
#27269=CARTESIAN_POINT('Ctrl Pts',(-0.0475862280670742,0.699755567657756,
4.96563476101538));
#27270=CARTESIAN_POINT('Ctrl Pts',(0.028738398930405,0.700850964995508,
4.96254287357644));
#27271=CARTESIAN_POINT('Ctrl Pts',(0.105765749697592,0.693258892245674,
4.98506844977587));
#27272=CARTESIAN_POINT('Ctrl Pts',(0.14822387585714,0.684346822022482,5.01626492020255));
#27273=CARTESIAN_POINT('Ctrl Pts',(0.179544791652671,0.67673552419273,5.04776834727921));
#27274=CARTESIAN_POINT('Ctrl Pts',(0.192309606221861,0.673146741630874,
5.06447161752956));
#27275=CARTESIAN_POINT('Ctrl Pts',(0.202776724457231,0.669982292593922,
5.0828895760763));
#27276=CARTESIAN_POINT('Ctrl Pts',(0.202776724457231,0.669982292593922,
5.0828895760763));
#27277=CARTESIAN_POINT('Ctrl Pts',(0.207628057237965,0.668515623831736,
5.09142598925544));
#27278=CARTESIAN_POINT('Ctrl Pts',(0.211985806665345,0.667140108961854,
5.10033074597365));
#27279=CARTESIAN_POINT('Ctrl Pts',(0.231462706037527,0.66080100427468,5.14789144672313));
#27280=CARTESIAN_POINT('Ctrl Pts',(0.236794050807431,0.658726504222929,
5.18991348571448));
#27281=CARTESIAN_POINT('Ctrl Pts',(0.229928314309894,0.66115513119461,5.24311976375499));
#27282=CARTESIAN_POINT('Ctrl Pts',(0.227321703930627,0.662060184763746,
5.25551407980518));
#27283=CARTESIAN_POINT('Ctrl Pts',(0.215583701847853,0.666020452558282,
5.29529098994732));
#27284=CARTESIAN_POINT('Ctrl Pts',(0.202453501259093,0.670296320458785,
5.32107996750068));
#27285=CARTESIAN_POINT('Ctrl Pts',(0.153783173631022,0.683700872584965,
5.38492528292425));
#27286=CARTESIAN_POINT('Ctrl Pts',(0.108362285081162,0.693443393568619,
5.41500017367323));
#27287=CARTESIAN_POINT('Ctrl Pts',(0.0574844932621232,0.697635673567799,
5.42785529611499));
#27288=CARTESIAN_POINT('Origin',(0.,0.,4.7));
#27289=CARTESIAN_POINT('',(-0.7,-8.57252759403147E-17,4.74));
#27290=CARTESIAN_POINT('Origin',(0.,0.,4.74));
#27291=CARTESIAN_POINT('',(-0.7,-8.57252759403147E-17,6.1));
#27292=CARTESIAN_POINT('',(-0.7,-8.57252759403147E-17,4.7));
#27293=CARTESIAN_POINT('Origin',(0.,0.,6.1));
#27294=CARTESIAN_POINT('Origin',(0.,3.5858062517663E-17,4.7106066017178));
#27295=CARTESIAN_POINT('',(-1.12,-1.37160441504504E-16,4.7));
#27296=CARTESIAN_POINT('',(-1.1456066017178,-6.85802207522518E-17,4.7106066017178));
#27297=CARTESIAN_POINT('Origin',(0.,0.,4.7));
#27298=CARTESIAN_POINT('Origin',(0.,0.,4.7));
#27299=CARTESIAN_POINT('',(-0.74,9.06238631369041E-17,4.7));
#27300=CARTESIAN_POINT('Origin',(0.,0.,4.7));
#27301=CARTESIAN_POINT('Origin',(0.,-1.3893933982822,5.7543933982822));
#27302=CARTESIAN_POINT('',(-2.8712132034356,-1.3787867965644,5.7287867965644));
#27303=CARTESIAN_POINT('',(2.8712132034356,-1.3787867965644,5.7287867965644));
#27304=CARTESIAN_POINT('',(0.,-1.3787867965644,5.7287867965644));
#27305=CARTESIAN_POINT('',(2.82,-1.4,5.78));
#27306=CARTESIAN_POINT('',(2.8712132034356,-1.3787867965644,5.7287867965644));
#27307=CARTESIAN_POINT('',(-2.82,-1.4,5.78));
#27308=CARTESIAN_POINT('',(0.,-1.4,5.78));
#27309=CARTESIAN_POINT('',(-2.82,-1.4,5.78));
#27310=CARTESIAN_POINT('Origin',(0.,-1.3893933982822,6.2456066017178));
#27311=CARTESIAN_POINT('',(-2.82,-1.4,6.22));
#27312=CARTESIAN_POINT('',(2.82,-1.4,6.22));
#27313=CARTESIAN_POINT('',(0.,-1.4,6.22));
#27314=CARTESIAN_POINT('',(2.82,-1.4,6.22));
#27315=CARTESIAN_POINT('',(-2.8712132034356,-1.3787867965644,6.2712132034356));
#27316=CARTESIAN_POINT('Origin',(2.8456066017178,-1.3893933982822,6.9375));
#27317=CARTESIAN_POINT('',(2.8712132034356,-1.3787867965644,6.9375));
#27318=CARTESIAN_POINT('',(2.82,-1.4,6.9375));
#27319=CARTESIAN_POINT('Origin',(-2.8456066017178,-1.3893933982822,6.9375));
#27320=CARTESIAN_POINT('',(-2.8712132034356,-1.3787867965644,6.9375));
#27321=CARTESIAN_POINT('',(-2.82,-1.4,6.9375));
#27322=CARTESIAN_POINT('Origin',(-2.875,-1.375,7.575));
#27323=CARTESIAN_POINT('',(-2.8787867965644,-1.3712132034356,5.7287867965644));
#27324=CARTESIAN_POINT('',(-2.8787867965644,-1.3712132034356,8.2125));
#27325=CARTESIAN_POINT('',(-2.875,-1.375,5.725));
#27326=CARTESIAN_POINT('',(-3.27916666666667,-0.970833333333332,6.12916666666666));
#27327=CARTESIAN_POINT('',(-2.0875,-2.1625,6.5125));
#27328=CARTESIAN_POINT('Origin',(0.,-1.4,6.3));
#27329=CARTESIAN_POINT('Origin',(2.885,0.4,11.985));
#27330=CARTESIAN_POINT('',(2.895,0.225,11.975));
#27331=CARTESIAN_POINT('',(2.9,0.23,11.97));
#27332=CARTESIAN_POINT('',(3.17583333333333,0.505833333333333,11.6941666666667));
#27333=CARTESIAN_POINT('',(2.9,0.95,11.97));
#27334=CARTESIAN_POINT('',(2.9,0.4,11.97));
#27335=CARTESIAN_POINT('',(2.885,0.965,11.985));
#27336=CARTESIAN_POINT('',(3.76083333333333,0.0891666666666678,11.1091666666667));
#27337=CARTESIAN_POINT('',(2.87,0.95,12.));
#27338=CARTESIAN_POINT('',(2.31333333333332,0.393333333333335,12.5566666666667));
#27339=CARTESIAN_POINT('',(2.87,0.25,12.));
#27340=CARTESIAN_POINT('',(2.87,0.4,12.));
#27341=CARTESIAN_POINT('',(2.37999999999999,0.74,12.49));
#27342=CARTESIAN_POINT('Origin',(2.885,0.215,10.425));
#27343=CARTESIAN_POINT('',(2.8912132034356,0.221213203435596,11.9712132034356));
#27344=CARTESIAN_POINT('',(2.15083333333334,-0.519166666666663,11.2308333333333));
#27345=CARTESIAN_POINT('',(2.87,0.2,11.92));
#27346=CARTESIAN_POINT('',(2.8912132034356,0.221213203435596,11.9712132034356));
#27347=CARTESIAN_POINT('',(2.87,0.2,6.4));
#27348=CARTESIAN_POINT('',(2.87,0.2,10.425));
#27349=CARTESIAN_POINT('',(2.9,0.23,6.4));
#27350=CARTESIAN_POINT('',(2.87,0.2,6.4));
#27351=CARTESIAN_POINT('',(2.9,0.23,10.425));
#27352=CARTESIAN_POINT('Origin',(0.,0.225,11.975));
#27353=CARTESIAN_POINT('',(-2.87,0.25,12.));
#27354=CARTESIAN_POINT('',(0.,0.25,12.));
#27355=CARTESIAN_POINT('',(-2.895,0.225,11.975));
#27356=CARTESIAN_POINT('',(-2.37999999999999,0.74,12.49));
#27357=CARTESIAN_POINT('',(-2.8912132034356,0.221213203435596,11.9712132034356));
#27358=CARTESIAN_POINT('',(-2.15083333333334,-0.519166666666663,11.2308333333333));
#27359=CARTESIAN_POINT('',(0.,0.221213203435596,11.9712132034356));
#27360=CARTESIAN_POINT('Origin',(0.,1.,12.));
#27361=CARTESIAN_POINT('',(-2.87,0.95,12.));
#27362=CARTESIAN_POINT('',(0.,0.95,12.));
#27363=CARTESIAN_POINT('',(-2.87,0.4,12.));
#27364=CARTESIAN_POINT('Origin',(2.8893933982822,-0.5,5.7543933982822));
#27365=CARTESIAN_POINT('',(2.8787867965644,0.971213203435596,5.7287867965644));
#27366=CARTESIAN_POINT('',(2.8787867965644,-0.5,5.7287867965644));
#27367=CARTESIAN_POINT('',(2.9,0.95,5.78));
#27368=CARTESIAN_POINT('',(3.2153138421172,0.6346861578828,6.54123495404334));
#27369=CARTESIAN_POINT('',(2.9,-0.5,5.78));
#27370=CARTESIAN_POINT('Origin',(2.875,0.975,7.275));
#27371=CARTESIAN_POINT('',(2.9,0.95,7.275));
#27372=CARTESIAN_POINT('',(2.875,0.975,5.725));
#27373=CARTESIAN_POINT('',(3.42916666666667,0.420833333333331,6.27916666666667));
#27374=CARTESIAN_POINT('',(2.8712132034356,0.978786796564403,5.7287867965644));
#27375=CARTESIAN_POINT('',(2.1375,1.7125,6.4625));
#27376=CARTESIAN_POINT('',(2.8712132034356,0.978786796564403,11.9712132034356));
#27377=CARTESIAN_POINT('',(2.8712132034356,0.978786796564403,6.4875));
#27378=CARTESIAN_POINT('',(1.61250000000001,2.2375,10.7125));
#27379=CARTESIAN_POINT('Origin',(2.875,-0.8,5.725));
#27380=CARTESIAN_POINT('',(2.1,0.199999999999996,4.95));
#27381=CARTESIAN_POINT('',(2.875,-1.375,5.725));
#27382=CARTESIAN_POINT('',(3.27916666666667,-0.970833333333332,6.12916666666666));
#27383=CARTESIAN_POINT('',(2.3,-0.8,5.15));
#27384=CARTESIAN_POINT('Origin',(2.875,-1.375,7.575));
#27385=CARTESIAN_POINT('',(2.0875,-2.1625,6.5125));
#27386=CARTESIAN_POINT('Origin',(-2.8893933982822,-0.5,5.7543933982822));
#27387=CARTESIAN_POINT('',(-2.9,-1.32,5.78));
#27388=CARTESIAN_POINT('',(-2.9,0.95,5.78));
#27389=CARTESIAN_POINT('',(-2.9,-0.5,5.78));
#27390=CARTESIAN_POINT('',(-2.8787867965644,0.971213203435596,5.7287867965644));
#27391=CARTESIAN_POINT('',(-3.2153138421172,0.6346861578828,6.54123495404334));
#27392=CARTESIAN_POINT('',(-2.8787867965644,-0.5,5.7287867965644));
#27393=CARTESIAN_POINT('',(-2.8787867965644,-1.3712132034356,5.7287867965644));
#27394=CARTESIAN_POINT('Origin',(-2.8893933982822,-1.3456066017178,8.2125));
#27395=CARTESIAN_POINT('',(-2.9,-1.32,6.27));
#27396=CARTESIAN_POINT('',(-2.97292879382193,-1.14393431686758,6.19707120617807));
#27397=CARTESIAN_POINT('',(-2.9,-1.32,8.2125));
#27398=CARTESIAN_POINT('Origin',(-2.875,0.975,7.275));
#27399=CARTESIAN_POINT('',(-2.9,0.95,11.97));
#27400=CARTESIAN_POINT('',(-2.9,0.95,7.275));
#27401=CARTESIAN_POINT('',(-2.885,0.965,11.985));
#27402=CARTESIAN_POINT('',(-3.76083333333333,0.0891666666666678,11.1091666666667));
#27403=CARTESIAN_POINT('',(-2.8712132034356,0.978786796564404,11.9712132034356));
#27404=CARTESIAN_POINT('',(-1.61250000000001,2.2375,10.7125));
#27405=CARTESIAN_POINT('',(-2.8712132034356,0.978786796564403,5.7287867965644));
#27406=CARTESIAN_POINT('',(-2.8712132034356,0.978786796564403,6.4875));
#27407=CARTESIAN_POINT('',(-2.875,0.975,5.725));
#27408=CARTESIAN_POINT('',(-2.1375,1.7125,6.4625));
#27409=CARTESIAN_POINT('',(-3.42916666666667,0.420833333333331,6.27916666666667));
#27410=CARTESIAN_POINT('Origin',(-2.9,-0.2,8.85));
#27411=CARTESIAN_POINT('',(-2.9,0.1,6.27));
#27412=CARTESIAN_POINT('',(-2.9,2.77555756156289E-17,6.27));
#27413=CARTESIAN_POINT('',(-2.9,0.23,6.4));
#27414=CARTESIAN_POINT('Origin',(-2.9,0.1,6.4));
#27415=CARTESIAN_POINT('',(-2.9,0.23,11.97));
#27416=CARTESIAN_POINT('',(-2.9,0.23,10.425));
#27417=CARTESIAN_POINT('',(-2.9,0.4,11.97));
#27418=CARTESIAN_POINT('Origin',(-2.885,2.77555756156289E-17,6.285));
#27419=CARTESIAN_POINT('',(-2.87,0.1,6.3));
#27420=CARTESIAN_POINT('',(-2.87,2.77555756156289E-17,6.3));
#27421=CARTESIAN_POINT('',(-2.87,0.1,6.3));
#27422=CARTESIAN_POINT('Origin',(-2.885,0.4,11.985));
#27423=CARTESIAN_POINT('',(-3.17583333333333,0.505833333333333,11.6941666666667));
#27424=CARTESIAN_POINT('',(-2.31333333333332,0.393333333333335,12.5566666666667));
#27425=CARTESIAN_POINT('Origin',(-2.885,0.215,10.425));
#27426=CARTESIAN_POINT('',(-2.87,0.2,6.4));
#27427=CARTESIAN_POINT('',(-2.87,0.2,6.4));
#27428=CARTESIAN_POINT('',(-2.87,0.2,11.92));
#27429=CARTESIAN_POINT('',(-2.87,0.2,10.425));
#27430=CARTESIAN_POINT('',(-2.87,0.2,11.92));
#27431=CARTESIAN_POINT('Origin',(2.1843933982822,0.210606601717798,11.35));
#27432=CARTESIAN_POINT('',(2.21,0.2,10.67));
#27433=CARTESIAN_POINT('',(2.21,0.2,11.53));
#27434=CARTESIAN_POINT('',(2.21,0.2,11.35));
#27435=CARTESIAN_POINT('',(2.1587867965644,0.221213203435596,11.5087867965644));
#27436=CARTESIAN_POINT('',(2.21,0.2,11.53));
#27437=CARTESIAN_POINT('',(2.1587867965644,0.221213203435596,10.6912132034356));
#27438=CARTESIAN_POINT('',(2.1587867965644,0.221213203435596,11.35));
#27439=CARTESIAN_POINT('',(2.1587867965644,0.221213203435596,10.6912132034356));
#27440=CARTESIAN_POINT('Origin',(1.8156066017178,0.210606601717798,11.35));
#27441=CARTESIAN_POINT('',(1.79,0.2,11.53));
#27442=CARTESIAN_POINT('',(1.79,0.2,10.67));
#27443=CARTESIAN_POINT('',(1.79,0.2,11.35));
#27444=CARTESIAN_POINT('',(1.8412132034356,0.221213203435597,10.6912132034356));
#27445=CARTESIAN_POINT('',(1.79,0.2,10.67));
#27446=CARTESIAN_POINT('',(1.8412132034356,0.221213203435597,11.5087867965644));
#27447=CARTESIAN_POINT('',(1.8412132034356,0.221213203435597,11.35));
#27448=CARTESIAN_POINT('',(1.8412132034356,0.221213203435597,11.5087867965644));
#27449=CARTESIAN_POINT('Origin',(1.,0.215,10.685));
#27450=CARTESIAN_POINT('',(2.15,0.23,10.7));
#27451=CARTESIAN_POINT('',(1.85,0.23,10.7));
#27452=CARTESIAN_POINT('',(1.,0.23,10.7));
#27453=CARTESIAN_POINT('',(1.75333333333333,0.133333333333332,10.6033333333333));
#27454=CARTESIAN_POINT('',(1.,0.2,10.67));
#27455=CARTESIAN_POINT('',(1.99,0.390000000000002,10.86));
#27456=CARTESIAN_POINT('Origin',(1.,0.215,11.515));
#27457=CARTESIAN_POINT('',(1.,0.2,11.53));
#27458=CARTESIAN_POINT('',(1.85,0.23,11.5));
#27459=CARTESIAN_POINT('',(1.88666666666666,0.266666666666665,11.4633333333333));
#27460=CARTESIAN_POINT('',(2.15,0.23,11.5));
#27461=CARTESIAN_POINT('',(1.,0.23,11.5));
#27462=CARTESIAN_POINT('',(1.85666666666667,0.523333333333335,11.2066666666667));
#27463=CARTESIAN_POINT('Origin',(2.,0.265,11.5));
#27464=CARTESIAN_POINT('',(2.,0.38,11.5));
#27465=CARTESIAN_POINT('',(2.,0.38,11.5));
#27466=CARTESIAN_POINT('',(2.23,0.15,11.5));
#27467=CARTESIAN_POINT('Origin',(2.,0.38,10.7));
#27468=CARTESIAN_POINT('',(2.,0.38,10.7));
#27469=CARTESIAN_POINT('',(2.,0.38,10.7));
#27470=CARTESIAN_POINT('',(2.,0.38,10.7));
#27471=CARTESIAN_POINT('Origin',(0.,0.2,12.));
#27472=CARTESIAN_POINT('',(0.,0.2,6.4));
#27473=CARTESIAN_POINT('',(0.,0.2,11.92));
#27474=CARTESIAN_POINT('',(1.79,0.2,7.3));
#27475=CARTESIAN_POINT('Origin',(2.,0.2,7.3));
#27476=CARTESIAN_POINT('',(1.7,0.2,9.765));
#27477=CARTESIAN_POINT('Origin',(1.7,0.2,10.));
#27478=CARTESIAN_POINT('',(-1.98,0.2,9.7));
#27479=CARTESIAN_POINT('Origin',(-0.4,0.2,9.7));
#27480=CARTESIAN_POINT('',(2.87791997799628E-17,0.2,7.065));
#27481=CARTESIAN_POINT('Origin',(0.,0.2,7.3));
#27482=CARTESIAN_POINT('Origin',(2.,0.210606601717798,7.3));
#27483=CARTESIAN_POINT('',(1.8412132034356,0.221213203435596,7.3));
#27484=CARTESIAN_POINT('',(1.8156066017178,0.210606601717798,7.3));
#27485=CARTESIAN_POINT('Origin',(2.,0.221213203435596,7.3));
#27486=CARTESIAN_POINT('Origin',(2.,0.265,7.3));
#27487=CARTESIAN_POINT('',(2.,0.38,7.3));
#27488=CARTESIAN_POINT('',(1.885,0.265,7.3));
#27489=CARTESIAN_POINT('Origin',(0.,0.215,7.3));
#27490=CARTESIAN_POINT('',(-2.51052593825207E-17,0.23,7.095));
#27491=CARTESIAN_POINT('',(2.69422295812418E-17,0.215,7.08));
#27492=CARTESIAN_POINT('Origin',(0.,0.23,7.3));
#27493=CARTESIAN_POINT('Origin',(0.,0.6,7.3));
#27494=CARTESIAN_POINT('',(2.51052593825207E-17,0.97,7.095));
#27495=CARTESIAN_POINT('',(-2.51052593825207E-17,0.6,7.095));
#27496=CARTESIAN_POINT('Origin',(0.,0.97,7.3));
#27497=CARTESIAN_POINT('Origin',(1.7,0.215,10.));
#27498=CARTESIAN_POINT('',(1.7,0.23,9.795));
#27499=CARTESIAN_POINT('',(1.7,0.215,9.78));
#27500=CARTESIAN_POINT('Origin',(1.7,0.23,10.));
#27501=CARTESIAN_POINT('Origin',(1.7,0.6,10.));
#27502=CARTESIAN_POINT('',(1.7,0.97,9.795));
#27503=CARTESIAN_POINT('',(1.7,0.6,9.795));
#27504=CARTESIAN_POINT('Origin',(1.7,0.97,10.));
#27505=CARTESIAN_POINT('Origin',(-2.885,0.1,6.4));
#27506=CARTESIAN_POINT('Origin',(-2.87,0.1,6.4));
#27507=CARTESIAN_POINT('Origin',(0.,0.210606601717798,11.9456066017178));
#27508=CARTESIAN_POINT('Origin',(2.885,0.1,6.4));
#27509=CARTESIAN_POINT('Origin',(2.87,0.1,6.4));
#27510=CARTESIAN_POINT('Origin',(2.9,0.1,6.4));
#27511=CARTESIAN_POINT('Origin',(2.9,-0.2,8.85));
#27512=CARTESIAN_POINT('Origin',(-0.4,0.210606601717798,9.7));
#27513=CARTESIAN_POINT('',(-1.9287867965644,0.221213203435596,9.7));
#27514=CARTESIAN_POINT('Origin',(-0.4,0.221213203435597,9.7));
#27515=CARTESIAN_POINT('',(-1.9543933982822,0.210606601717798,9.7));
#27516=CARTESIAN_POINT('Origin',(-0.4,0.225,9.7));
#27517=CARTESIAN_POINT('',(-1.9212132034356,0.228786796564403,9.7));
#27518=CARTESIAN_POINT('',(-1.925,0.225,9.7));
#27519=CARTESIAN_POINT('Origin',(-0.4,0.228786796564403,9.7));
#27520=CARTESIAN_POINT('Origin',(0.,0.985,7.3));
#27521=CARTESIAN_POINT('',(-2.87791997799628E-17,1.,7.065));
#27522=CARTESIAN_POINT('Origin',(0.,1.,7.3));
#27523=CARTESIAN_POINT('',(-2.69422295812418E-17,0.985,7.08));
#27524=CARTESIAN_POINT('Origin',(0.,1.,5.7));
#27525=CARTESIAN_POINT('',(-2.82,1.,5.78));
#27526=CARTESIAN_POINT('',(2.82,1.,5.78));
#27527=CARTESIAN_POINT('',(0.,1.,5.78));
#27528=CARTESIAN_POINT('',(-2.82,1.,11.92));
#27529=CARTESIAN_POINT('',(-2.82,1.,6.4875));
#27530=CARTESIAN_POINT('',(2.82,1.,11.92));
#27531=CARTESIAN_POINT('',(0.,1.,11.92));
#27532=CARTESIAN_POINT('',(2.82,1.,6.4875));
#27533=CARTESIAN_POINT('',(1.7,1.,9.765));
#27534=CARTESIAN_POINT('Origin',(1.7,1.,10.));
#27535=CARTESIAN_POINT('',(-1.98,1.,9.7));
#27536=CARTESIAN_POINT('Origin',(-0.4,1.,9.7));
#27537=CARTESIAN_POINT('Origin',(1.7,0.985,10.));
#27538=CARTESIAN_POINT('',(1.7,0.985,9.78));
#27539=CARTESIAN_POINT('Origin',(0.,0.989393398282202,11.9456066017178));
#27540=CARTESIAN_POINT('',(0.,0.978786796564404,11.9712132034356));
#27541=CARTESIAN_POINT('',(2.8712132034356,0.978786796564404,11.9712132034356));
#27542=CARTESIAN_POINT('',(-2.82,1.,11.92));
#27543=CARTESIAN_POINT('Origin',(0.,0.989393398282202,5.7543933982822));
#27544=CARTESIAN_POINT('',(2.82,1.,5.78));
#27545=CARTESIAN_POINT('',(0.,0.978786796564403,5.7287867965644));
#27546=CARTESIAN_POINT('',(-2.8712132034356,0.978786796564403,5.7287867965644));
#27547=CARTESIAN_POINT('Origin',(2.8456066017178,0.989393398282202,6.4875));
#27548=CARTESIAN_POINT('Origin',(-2.8456066017178,0.989393398282202,6.4875));
#27549=CARTESIAN_POINT('Origin',(0.,0.975,5.725));
#27550=CARTESIAN_POINT('',(0.,0.95,5.7));
#27551=CARTESIAN_POINT('',(-2.1,0.199999999999996,4.95));
#27552=CARTESIAN_POINT('Origin',(-0.4,0.254393398282202,9.7));
#27553=CARTESIAN_POINT('',(-1.9,0.28,9.7));
#27554=CARTESIAN_POINT('',(-1.9106066017178,0.254393398282202,9.7));
#27555=CARTESIAN_POINT('Origin',(-0.4,0.28,9.7));
#27556=CARTESIAN_POINT('Origin',(-0.4,1.,9.7));
#27557=CARTESIAN_POINT('',(-1.9,0.92,9.7));
#27558=CARTESIAN_POINT('Origin',(-0.4,0.92,9.7));
#27559=CARTESIAN_POINT('',(-1.9,1.,9.7));
#27560=CARTESIAN_POINT('Origin',(-0.4,0.989393398282202,9.7));
#27561=CARTESIAN_POINT('',(-1.9287867965644,0.978786796564403,9.7));
#27562=CARTESIAN_POINT('Origin',(-0.4,0.978786796564403,9.7));
#27563=CARTESIAN_POINT('',(-1.9543933982822,0.989393398282202,9.7));
#27564=CARTESIAN_POINT('Origin',(-0.4,0.975,9.7));
#27565=CARTESIAN_POINT('',(-1.9212132034356,0.971213203435596,9.7));
#27566=CARTESIAN_POINT('',(-1.925,0.975,9.7));
#27567=CARTESIAN_POINT('Origin',(-0.4,0.971213203435596,9.7));
#27568=CARTESIAN_POINT('Origin',(-0.4,0.945606601717798,9.7));
#27569=CARTESIAN_POINT('',(-1.9106066017178,0.945606601717798,9.7));
#27570=CARTESIAN_POINT('Origin',(2.23,0.15,10.7));
#27571=CARTESIAN_POINT('',(2.23,0.15,10.7));
#27572=CARTESIAN_POINT('Origin',(2.,0.265,10.7));
#27573=CARTESIAN_POINT('Origin',(0.,0.,4.72));
#27574=CARTESIAN_POINT('',(-0.72,8.81745695386094E-17,4.72));
#27575=CARTESIAN_POINT('Origin',(0.,0.,6.1));
#27576=CARTESIAN_POINT('Origin',(0.,0.,5.7));
#27577=CARTESIAN_POINT('Origin',(0.,-1.375,5.725));
#27578=CARTESIAN_POINT('',(-2.3,-0.8,5.15));
#27579=CARTESIAN_POINT('Origin',(-2.875,-0.8,5.725));
#27580=CARTESIAN_POINT('Origin',(0.,0.975,11.975));
#27581=CARTESIAN_POINT('Origin',(0.,0.2,6.3));
#27582=CARTESIAN_POINT('',(0.,0.1,6.3));
#27583=CARTESIAN_POINT('Origin',(0.,0.1,6.4));
#27584=CARTESIAN_POINT('',(0.,0.,0.));
#27585=CARTESIAN_POINT('Origin',(0.,0.,-0.58));
#27586=CARTESIAN_POINT('',(-0.246625721155034,0.000168494669343964,-1.14757872191302));
#27587=CARTESIAN_POINT('',(-0.246561196381942,0.00027133617513674,-1.15472127808698));
#27588=CARTESIAN_POINT('',(-0.24635,-3.0169173896995E-17,-0.58));
#27589=CARTESIAN_POINT('',(0.107012561312306,0.222107835256874,-1.16365));
#27590=CARTESIAN_POINT('Ctrl Pts',(-0.246625721155034,0.000168494669343964,
-1.14757872191302));
#27591=CARTESIAN_POINT('Ctrl Pts',(-0.246691802496828,0.00929404761416736,
-1.147874469355));
#27592=CARTESIAN_POINT('Ctrl Pts',(-0.246229090033986,0.0184124162622834,
-1.14817021679697));
#27593=CARTESIAN_POINT('Ctrl Pts',(-0.245215256688347,0.0274685625149367,
-1.14846596423895));
#27594=CARTESIAN_POINT('Ctrl Pts',(-0.236164717639783,0.108313215772521,
-1.15110611588088));
#27595=CARTESIAN_POINT('Ctrl Pts',(-0.183194149645427,0.184199230199488,
-1.15374626752281));
#27596=CARTESIAN_POINT('Ctrl Pts',(-0.11042968587659,0.220635087366368,
-1.15638641916474));
#27597=CARTESIAN_POINT('Ctrl Pts',(-0.0436998617096857,0.254049177379322,
-1.15880761277649));
#27598=CARTESIAN_POINT('Ctrl Pts',(0.0396768319088052,0.254285280338311,
-1.16122880638824));
#27599=CARTESIAN_POINT('Ctrl Pts',(0.107142060752371,0.222259968661296,
-1.16365));
#27600=CARTESIAN_POINT('',(-0.106883061872245,0.22195570185245,-1.16365));
#27601=CARTESIAN_POINT('Origin',(0.,0.,-1.16365));
#27602=CARTESIAN_POINT('Ctrl Pts',(-0.106883061872243,0.221955701852451,
-1.16365));
#27603=CARTESIAN_POINT('Ctrl Pts',(-0.180521580324393,0.186494975868788,
-1.16100984835807));
#27604=CARTESIAN_POINT('Ctrl Pts',(-0.234503589708069,0.111829210743298,
-1.15836969671614));
#27605=CARTESIAN_POINT('Ctrl Pts',(-0.244745176790073,0.0312497853638165,
-1.15572954507421));
#27606=CARTESIAN_POINT('Ctrl Pts',(-0.246048921871434,0.0209920949632681,
-1.15539345607847));
#27607=CARTESIAN_POINT('Ctrl Pts',(-0.246643850461073,0.0106385732996934,
-1.15505736708273));
#27608=CARTESIAN_POINT('Ctrl Pts',(-0.246561196381942,0.00027133617513674,
-1.15472127808698));
#27609=CARTESIAN_POINT('Origin',(0.,0.,-0.58));
#27610=CARTESIAN_POINT('',(-0.245986779925945,9.73375077604199E-5,-1.09757872191302));
#27611=CARTESIAN_POINT('',(-0.245972779806236,8.0061809554402E-5,-1.10472127808698));
#27612=CARTESIAN_POINT('',(-0.24635,-3.0169173896995E-17,-0.58));
#27613=CARTESIAN_POINT('Ctrl Pts',(-0.245986779925945,9.73375077604199E-5,
-1.09757872191302));
#27614=CARTESIAN_POINT('Ctrl Pts',(-0.246110835529417,0.0349354674350985,
-1.09870022617009));
#27615=CARTESIAN_POINT('Ctrl Pts',(-0.239203249496549,0.0697265760046414,
-1.09982173042716));
#27616=CARTESIAN_POINT('Ctrl Pts',(-0.225022115887616,0.1012449175221,-1.10094323468424));
#27617=CARTESIAN_POINT('Ctrl Pts',(-0.191638075705932,0.175442764372367,
-1.10358338632616));
#27618=CARTESIAN_POINT('Ctrl Pts',(-0.117945021508019,0.231503380167954,
-1.10622353796809));
#27619=CARTESIAN_POINT('Ctrl Pts',(-0.0375289851653269,0.243878547528516,
-1.10886368961002));
#27620=CARTESIAN_POINT('Ctrl Pts',(0.0428870511773651,0.256253714889078,
-1.11150384125195));
#27621=CARTESIAN_POINT('Ctrl Pts',(0.130026069664836,0.224943433814618,
-1.11414399289388));
#27622=CARTESIAN_POINT('Ctrl Pts',(0.184172931613497,0.164213916417055,
-1.11678414453581));
#27623=CARTESIAN_POINT('Ctrl Pts',(0.238319793562158,0.103484399019491,
-1.11942429617774));
#27624=CARTESIAN_POINT('Ctrl Pts',(0.259474498972009,0.013335645298826,
-1.12206444781966));
#27625=CARTESIAN_POINT('Ctrl Pts',(0.237996781658196,-0.065138960392713,
-1.12470459946159));
#27626=CARTESIAN_POINT('Ctrl Pts',(0.216519064344383,-0.143613566084252,
-1.12734475110352));
#27627=CARTESIAN_POINT('Ctrl Pts',(0.152408924306906,-0.210414023746664,
-1.12998490274545));
#27628=CARTESIAN_POINT('Ctrl Pts',(0.074882920919521,-0.235108951496199,
-1.13262505438738));
#27629=CARTESIAN_POINT('Ctrl Pts',(-0.00264308246786443,-0.259803879245735,
-1.13526520602931));
#27630=CARTESIAN_POINT('Ctrl Pts',(-0.0935849492051585,-0.242393277082393,
-1.13790535767124));
#27631=CARTESIAN_POINT('Ctrl Pts',(-0.15649062752242,-0.190786329956621,
-1.14054550931316));
#27632=CARTESIAN_POINT('Ctrl Pts',(-0.212349667626659,-0.144960347211201,
-1.14288991351311));
#27633=CARTESIAN_POINT('Ctrl Pts',(-0.24610189117968,-0.0721702025233373,
-1.14523431771307));
#27634=CARTESIAN_POINT('Ctrl Pts',(-0.246625721155034,0.000168494669343964,
-1.14757872191302));
#27635=CARTESIAN_POINT('Ctrl Pts',(-0.246561196381942,0.00027133617513674,
-1.15472127808698));
#27636=CARTESIAN_POINT('Ctrl Pts',(-0.245994560226962,-0.0708013978486803,
-1.1524172154408));
#27637=CARTESIAN_POINT('Ctrl Pts',(-0.213582849563037,-0.142518732003264,
-1.15011315279461));
#27638=CARTESIAN_POINT('Ctrl Pts',(-0.159389473178768,-0.188423293933392,
-1.14780909014843));
#27639=CARTESIAN_POINT('Ctrl Pts',(-0.0972910177051287,-0.241023862217646,
-1.1451689385065));
#27640=CARTESIAN_POINT('Ctrl Pts',(-0.00659294197751922,-0.259731913152679,
-1.14252878686457));
#27641=CARTESIAN_POINT('Ctrl Pts',(0.0713071689350544,-0.236198721659865,
-1.13988863522264));
#27642=CARTESIAN_POINT('Ctrl Pts',(0.149207279847628,-0.212665530167051,
-1.13724848358071));
#27643=CARTESIAN_POINT('Ctrl Pts',(0.214309425945166,-0.146891096246389,
-1.13460833193878));
#27644=CARTESIAN_POINT('Ctrl Pts',(0.236974179897325,-0.0687624955230583,
-1.13196818029685));
#27645=CARTESIAN_POINT('Ctrl Pts',(0.259638933849485,0.00936610520027226,
-1.12932802865493));
#27646=CARTESIAN_POINT('Ctrl Pts',(0.239866295656266,0.0998488727262715,
-1.126687877013));
#27647=CARTESIAN_POINT('Ctrl Pts',(0.186651310767665,0.161400207752535,
-1.12404772537107));
#27648=CARTESIAN_POINT('Ctrl Pts',(0.133436325879063,0.222951542778798,
-1.12140757372914));
#27649=CARTESIAN_POINT('Ctrl Pts',(0.0467789942950804,0.255571445305326,
-1.11876742208721));
#27650=CARTESIAN_POINT('Ctrl Pts',(-0.0338170183009678,0.244417831018811,
-1.11612727044528));
#27651=CARTESIAN_POINT('Ctrl Pts',(-0.114413030897016,0.233264216732296,
-1.11348711880335));
#27652=CARTESIAN_POINT('Ctrl Pts',(-0.188947724505129,0.178337085632739,
-1.11084696716143));
#27653=CARTESIAN_POINT('Ctrl Pts',(-0.22345572321461,0.104657009211454,
-1.1082068155195));
#27654=CARTESIAN_POINT('Ctrl Pts',(-0.238641583414576,0.0722327776738232,
-1.10704496970866));
#27655=CARTESIAN_POINT('Ctrl Pts',(-0.246075885996451,0.0361768564216556,
-1.10588312389782));
#27656=CARTESIAN_POINT('Ctrl Pts',(-0.245972779806236,8.0061809554402E-5,
-1.10472127808698));
#27657=CARTESIAN_POINT('Origin',(0.,0.,-0.58));
#27658=CARTESIAN_POINT('',(-0.246278037043403,-0.000220690792281708,-1.04757872191302));
#27659=CARTESIAN_POINT('',(-0.246314807272961,-0.000222469138248099,-1.05472127808698));
#27660=CARTESIAN_POINT('',(-0.24635,-3.0169173896995E-17,-0.58));
#27661=CARTESIAN_POINT('Ctrl Pts',(-0.246278037043403,-0.000220690792281708,
-1.04757872191302));
#27662=CARTESIAN_POINT('Ctrl Pts',(-0.245746501286765,0.0600881005582325,
-1.04952598298519));
#27663=CARTESIAN_POINT('Ctrl Pts',(-0.22339687683019,0.120749402095025,
-1.05147324405735));
#27664=CARTESIAN_POINT('Ctrl Pts',(-0.183195388910587,0.165302445288965,
-1.05342050512952));
#27665=CARTESIAN_POINT('Ctrl Pts',(-0.128689074448717,0.22570872148,-1.05606065677145));
#27666=CARTESIAN_POINT('Ctrl Pts',(-0.0413662088476531,0.256503664111021,
-1.05870080841338));
#27667=CARTESIAN_POINT('Ctrl Pts',(0.0389749219358994,0.243652203884091,
-1.0613409600553));
#27668=CARTESIAN_POINT('Ctrl Pts',(0.119316052719451,0.23080074365716,-1.06398111169723));
#27669=CARTESIAN_POINT('Ctrl Pts',(0.192675448685492,0.174302880572279,
-1.06662126333916));
#27670=CARTESIAN_POINT('Ctrl Pts',(0.225618797988557,0.0999080160201263,
-1.06926141498109));
#27671=CARTESIAN_POINT('Ctrl Pts',(0.258562147291622,0.0255131514679726,
-1.07190156662302));
#27672=CARTESIAN_POINT('Ctrl Pts',(0.25108944993171,-0.0667787145514542,
-1.07454171826495));
#27673=CARTESIAN_POINT('Ctrl Pts',(0.206606490170236,-0.134904463759243,
-1.07718186990688));
#27674=CARTESIAN_POINT('Ctrl Pts',(0.162123530408764,-0.203030212967032,
-1.07982202154881));
#27675=CARTESIAN_POINT('Ctrl Pts',(0.0806303082457299,-0.246989845363183,
-1.08246217319073));
#27676=CARTESIAN_POINT('Ctrl Pts',(-0.000731851916270801,-0.24674859612438,
-1.08510232483266));
#27677=CARTESIAN_POINT('Ctrl Pts',(-0.0820940120782718,-0.246507346885578,
-1.08774247647459));
#27678=CARTESIAN_POINT('Ctrl Pts',(-0.16332511023924,-0.202065216011821,
-1.09038262811652));
#27679=CARTESIAN_POINT('Ctrl Pts',(-0.207403146236997,-0.133676611622469,
-1.09302277975845));
#27680=CARTESIAN_POINT('Ctrl Pts',(-0.232757369469678,-0.0943386533171701,
-1.0945414271433));
#27681=CARTESIAN_POINT('Ctrl Pts',(-0.245818794190178,-0.0470775479853526,
-1.09606007452816));
#27682=CARTESIAN_POINT('Ctrl Pts',(-0.245986779925945,9.73375077604199E-5,
-1.09757872191302));
#27683=CARTESIAN_POINT('Ctrl Pts',(-0.245972779806236,8.0061809554402E-5,
-1.10472127808698));
#27684=CARTESIAN_POINT('Ctrl Pts',(-0.245841589866234,-0.0458486676835616,
-1.10324297225589));
#27685=CARTESIAN_POINT('Ctrl Pts',(-0.233507763949213,-0.0918435688210061,
-1.1017646664248));
#27686=CARTESIAN_POINT('Ctrl Pts',(-0.209412428525571,-0.130507897824181,
-1.10028636059371));
#27687=CARTESIAN_POINT('Ctrl Pts',(-0.166379831316204,-0.199559706695517,
-1.09764620895178));
#27688=CARTESIAN_POINT('Ctrl Pts',(-0.0858333330866237,-0.245230302695177,
-1.09500605730986));
#27689=CARTESIAN_POINT('Ctrl Pts',(-0.00448409557601711,-0.2467084525501,
-1.09236590566793));
#27690=CARTESIAN_POINT('Ctrl Pts',(0.0768651419345896,-0.248186602405022,
-1.089725754026));
#27691=CARTESIAN_POINT('Ctrl Pts',(0.159017118726222,-0.205472306115207,
-1.08708560238407));
#27692=CARTESIAN_POINT('Ctrl Pts',(0.204530894665673,-0.138031142950934,
-1.08444545074214));
#27693=CARTESIAN_POINT('Ctrl Pts',(0.250044670605124,-0.0705899797866627,
-1.08180529910021));
#27694=CARTESIAN_POINT('Ctrl Pts',(0.258920245692393,0.0215780502520655,
-1.07916514745828));
#27695=CARTESIAN_POINT('Ctrl Pts',(0.2271121342129,0.0964654205629691,-1.07652499581635));
#27696=CARTESIAN_POINT('Ctrl Pts',(0.195304022733407,0.171352790873873,
-1.07388484417443));
#27697=CARTESIAN_POINT('Ctrl Pts',(0.122812224687151,0.228959501456952,
-1.0712446925325));
#27698=CARTESIAN_POINT('Ctrl Pts',(0.0426758065862595,0.243031228537435,
-1.06860454089057));
#27699=CARTESIAN_POINT('Ctrl Pts',(-0.0374606115146319,0.257102955617917,
-1.06596438924864));
#27700=CARTESIAN_POINT('Ctrl Pts',(-0.125241649670159,0.227639699195803,
-1.06332423760671));
#27701=CARTESIAN_POINT('Ctrl Pts',(-0.180660295253063,0.168069364017089,
-1.06068408596478));
#27702=CARTESIAN_POINT('Ctrl Pts',(-0.22238147661892,0.123222639022737,
-1.05869648333885));
#27703=CARTESIAN_POINT('Ctrl Pts',(-0.245760855967737,0.0613123401091911,
-1.05670888071292));
#27704=CARTESIAN_POINT('Ctrl Pts',(-0.246314807272961,-0.000222469138248099,
-1.05472127808698));
#27705=CARTESIAN_POINT('Origin',(0.,0.,-0.58));
#27706=CARTESIAN_POINT('',(-0.246722231227711,7.40581688979149E-5,-0.997578721913017));
#27707=CARTESIAN_POINT('',(-0.246704275548887,9.50529893469801E-5,-1.00472127808698));
#27708=CARTESIAN_POINT('',(-0.24635,-3.0169173896995E-17,-0.58));
#27709=CARTESIAN_POINT('Ctrl Pts',(-0.246722231227711,7.40581688979149E-5,
-0.997578721913017));
#27710=CARTESIAN_POINT('Ctrl Pts',(-0.246738504101205,0.0041698706903469,
-0.997711588158351));
#27711=CARTESIAN_POINT('Ctrl Pts',(-0.246645299597814,0.00826492716717819,
-0.997844454403685));
#27712=CARTESIAN_POINT('Ctrl Pts',(-0.246440289964872,0.0123543787050153,
-0.997977320649018));
#27713=CARTESIAN_POINT('Ctrl Pts',(-0.242366595267892,0.0936148385388302,
-1.00061747229095));
#27714=CARTESIAN_POINT('Ctrl Pts',(-0.194147023620069,0.172662207183106,
-1.00325762393288));
#27715=CARTESIAN_POINT('Ctrl Pts',(-0.1237581402402,0.213469833851227,-1.0058977755748));
#27716=CARTESIAN_POINT('Ctrl Pts',(-0.0533692568603309,0.254277460519347,
-1.00853792721673));
#27717=CARTESIAN_POINT('Ctrl Pts',(0.0391889382515836,0.256845345211314,
-1.01117807885866));
#27718=CARTESIAN_POINT('Ctrl Pts',(0.111732096971909,0.220003148994786,
-1.01381823050059));
#27719=CARTESIAN_POINT('Ctrl Pts',(0.184275255692235,0.183160952778257,
-1.01645838214252));
#27720=CARTESIAN_POINT('Ctrl Pts',(0.236803378020971,0.106908675653232,
-1.01909853378445));
#27721=CARTESIAN_POINT('Ctrl Pts',(0.245376232297069,0.0259990745584446,
-1.02173868542638));
#27722=CARTESIAN_POINT('Ctrl Pts',(0.253949086573167,-0.0549105265363425,
-1.02437883706831));
#27723=CARTESIAN_POINT('Ctrl Pts',(0.218566672796627,-0.140477451600892,
-1.02701898871023));
#27724=CARTESIAN_POINT('Ctrl Pts',(0.155354890075996,-0.191703692271305,
-1.02965914035216));
#27725=CARTESIAN_POINT('Ctrl Pts',(0.0921431073553662,-0.242929932941718,
-1.03229929199409));
#27726=CARTESIAN_POINT('Ctrl Pts',(0.00110195569064579,-0.259815489217995,
-1.03493944363602));
#27727=CARTESIAN_POINT('Ctrl Pts',(-0.0762756258156698,-0.234664601507783,
-1.03757959527795));
#27728=CARTESIAN_POINT('Ctrl Pts',(-0.153653207321985,-0.209513713797572,
-1.04021974691988));
#27729=CARTESIAN_POINT('Ctrl Pts',(-0.217367218669897,-0.142326382100871,
-1.0428598985618));
#27730=CARTESIAN_POINT('Ctrl Pts',(-0.238379342682514,-0.0637239113769959,
-1.04550005020373));
#27731=CARTESIAN_POINT('Ctrl Pts',(-0.243893837512198,-0.0430952058664597,
-1.04619294077349));
#27732=CARTESIAN_POINT('Ctrl Pts',(-0.246467172500651,-0.0216802646510429,
-1.04688583134326));
#27733=CARTESIAN_POINT('Ctrl Pts',(-0.246278037043403,-0.000220690792281708,
-1.04757872191302));
#27734=CARTESIAN_POINT('Ctrl Pts',(-0.246314807272961,-0.000222469138248099,
-1.05472127808698));
#27735=CARTESIAN_POINT('Ctrl Pts',(-0.246496674802424,-0.0204249375290262,
-1.05406872907099));
#27736=CARTESIAN_POINT('Ctrl Pts',(-0.244218253557143,-0.0405869329434031,
-1.05341618005499));
#27737=CARTESIAN_POINT('Ctrl Pts',(-0.23932087891077,-0.0600913293117114,
-1.052763631039));
#27738=CARTESIAN_POINT('Ctrl Pts',(-0.21950656397529,-0.139004273526488,
-1.05012347939707));
#27739=CARTESIAN_POINT('Ctrl Pts',(-0.156821681094049,-0.20715274802073,
-1.04748332775514));
#27740=CARTESIAN_POINT('Ctrl Pts',(-0.0798355365549801,-0.233477462201628,
-1.04484317611321));
#27741=CARTESIAN_POINT('Ctrl Pts',(-0.00284939201591072,-0.259802176382527,
-1.04220302447128));
#27742=CARTESIAN_POINT('Ctrl Pts',(0.0884380141809866,-0.244303130250082,
-1.03956287282935));
#27743=CARTESIAN_POINT('Ctrl Pts',(0.152421523049327,-0.194044132905792,
-1.03692272118743));
#27744=CARTESIAN_POINT('Ctrl Pts',(0.216405031917667,-0.143785135561503,
-1.0342825695455));
#27745=CARTESIAN_POINT('Ctrl Pts',(0.253084643457451,-0.0587661870053685,
-1.03164241790357));
#27746=CARTESIAN_POINT('Ctrl Pts',(0.245743240432631,0.0222644322950805,
-1.02900226626164));
#27747=CARTESIAN_POINT('Ctrl Pts',(0.238401837407811,0.103295051595529,
-1.02636211461971));
#27748=CARTESIAN_POINT('Ctrl Pts',(0.187039419818387,0.180337341640293,
-1.02372196297778));
#27749=CARTESIAN_POINT('Ctrl Pts',(0.115064941057801,0.218278498474838,
-1.02108181133585));
#27750=CARTESIAN_POINT('Ctrl Pts',(0.0430904622972144,0.256219655309383,
-1.01844165969393));
#27751=CARTESIAN_POINT('Ctrl Pts',(-0.0494960776345338,0.255059678933708,
-1.015801508052));
#27752=CARTESIAN_POINT('Ctrl Pts',(-0.12049741408824,0.215327234607512,
-1.01316135641007));
#27753=CARTESIAN_POINT('Ctrl Pts',(-0.191498750541946,0.175594790281315,
-1.01052120476814));
#27754=CARTESIAN_POINT('Ctrl Pts',(-0.240914883517609,0.0972898780045968,
-1.00788105312621));
#27755=CARTESIAN_POINT('Ctrl Pts',(-0.246223901669846,0.0161007690757402,
-1.00524090148428));
#27756=CARTESIAN_POINT('Ctrl Pts',(-0.246572201114063,0.0107743375764552,
-1.00506769368518));
#27757=CARTESIAN_POINT('Ctrl Pts',(-0.246730661403056,0.00543549235529937,
-1.00489448588608));
#27758=CARTESIAN_POINT('Ctrl Pts',(-0.246704275548887,9.50529893469801E-5,
-1.00472127808698));
#27759=CARTESIAN_POINT('Origin',(0.,0.,-0.58));
#27760=CARTESIAN_POINT('',(-0.246068967124758,0.000163257868156283,-0.947578721913017));
#27761=CARTESIAN_POINT('',(-0.246044690514741,0.000148590017213961,-0.954721278086983));
#27762=CARTESIAN_POINT('',(-0.24635,-3.0169173896995E-17,-0.58));
#27763=CARTESIAN_POINT('Ctrl Pts',(-0.246068967124758,0.000163257868156283,
-0.947578721913017));
#27764=CARTESIAN_POINT('Ctrl Pts',(-0.246251016085628,0.0299166900142917,
-0.948537344973446));
#27765=CARTESIAN_POINT('Ctrl Pts',(-0.241256522550863,0.059611081389455,
-0.949495968033874));
#27766=CARTESIAN_POINT('Ctrl Pts',(-0.230811068104658,0.0872450458601642,
-0.950454591094303));
#27767=CARTESIAN_POINT('Ctrl Pts',(-0.202043156247306,0.163351974309931,
-0.953094742736232));
#27768=CARTESIAN_POINT('Ctrl Pts',(-0.131929095164112,0.22383033384413,
-0.955734894378161));
#27769=CARTESIAN_POINT('Ctrl Pts',(-0.0524240884788059,0.24111649079944,
-0.958375046020089));
#27770=CARTESIAN_POINT('Ctrl Pts',(0.0270809182064996,0.25840264775475,
-0.961015197662018));
#27771=CARTESIAN_POINT('Ctrl Pts',(0.115976870493916,0.232496602131172,
-0.963655349303947));
#27772=CARTESIAN_POINT('Ctrl Pts',(0.173748524901487,0.175205300374098,
-0.966295500945875));
#27773=CARTESIAN_POINT('Ctrl Pts',(0.231520179309058,0.117913998617024,
-0.968935652587804));
#27774=CARTESIAN_POINT('Ctrl Pts',(0.258167535836783,0.0292374407264532,
-0.971575804229732));
#27775=CARTESIAN_POINT('Ctrl Pts',(0.241545787992139,-0.0504091210988275,
-0.974215955871661));
#27776=CARTESIAN_POINT('Ctrl Pts',(0.224924040147495,-0.130055682924108,
-0.976856107513589));
#27777=CARTESIAN_POINT('Ctrl Pts',(0.165033187930483,-0.200672248684099,
-0.979496259155518));
#27778=CARTESIAN_POINT('Ctrl Pts',(0.0891691025107115,-0.23007459301933,
-0.982136410797447));
#27779=CARTESIAN_POINT('Ctrl Pts',(0.0133050170909386,-0.259476937354563,
-0.984776562439376));
#27780=CARTESIAN_POINT('Ctrl Pts',(-0.0785323015315946,-0.247665060265035,
-0.987416714081304));
#27781=CARTESIAN_POINT('Ctrl Pts',(-0.144487051969792,-0.200022346208593,
-0.990056865723233));
#27782=CARTESIAN_POINT('Ctrl Pts',(-0.20712261425475,-0.15477726281611,
-0.992564151119827));
#27783=CARTESIAN_POINT('Ctrl Pts',(-0.24641514993727,-0.0772169866440894,
-0.995071436516422));
#27784=CARTESIAN_POINT('Ctrl Pts',(-0.246722231227711,7.40581688979149E-5,
-0.997578721913017));
#27785=CARTESIAN_POINT('Ctrl Pts',(-0.246704275548887,9.50529893469801E-5,
-1.00472127808698));
#27786=CARTESIAN_POINT('Ctrl Pts',(-0.246328470182043,-0.0759671340501024,
-1.00225433424415));
#27787=CARTESIAN_POINT('Ctrl Pts',(-0.208455879730509,-0.152352699786071,
-0.999787390401325));
#27788=CARTESIAN_POINT('Ctrl Pts',(-0.147512243360909,-0.197801876593369,
-0.997320446558496));
#27789=CARTESIAN_POINT('Ctrl Pts',(-0.0822896635709238,-0.246442107752627,
-0.994680294916568));
#27790=CARTESIAN_POINT('Ctrl Pts',(0.00935739933785658,-0.259649264490148,
-0.99204014327464));
#27791=CARTESIAN_POINT('Ctrl Pts',(0.0856598552539378,-0.231404048586573,
-0.989399991632711));
#27792=CARTESIAN_POINT('Ctrl Pts',(0.161962311170019,-0.203158832682998,
-0.986759839990783));
#27793=CARTESIAN_POINT('Ctrl Pts',(0.222920160093402,-0.133461244138326,
-0.984119688348854));
#27794=CARTESIAN_POINT('Ctrl Pts',(0.240751235997126,-0.0540766753887532,
-0.981479536706925));
#27795=CARTESIAN_POINT('Ctrl Pts',(0.25858231190085,0.02530789336082,-0.978839385064996));
#27796=CARTESIAN_POINT('Ctrl Pts',(0.233286614784916,0.114379442315294,
-0.976199233423067));
#27797=CARTESIAN_POINT('Ctrl Pts',(0.176392918556739,0.172542698242494,
-0.973559081781138));
#27798=CARTESIAN_POINT('Ctrl Pts',(0.119499222328562,0.230705954169694,
-0.97091893013921));
#27799=CARTESIAN_POINT('Ctrl Pts',(0.0310075269881437,0.257960917069619,
-0.968278778497282));
#27800=CARTESIAN_POINT('Ctrl Pts',(-0.0487511682798576,0.241885857484542,
-0.965638626855353));
#27801=CARTESIAN_POINT('Ctrl Pts',(-0.128509863547858,0.225810797899465,
-0.962998475213425));
#27802=CARTESIAN_POINT('Ctrl Pts',(-0.199535558743442,0.166405715829386,
-0.960358323571496));
#27803=CARTESIAN_POINT('Ctrl Pts',(-0.229457563609463,0.0907450877634371,
-0.957718171929567));
#27804=CARTESIAN_POINT('Ctrl Pts',(-0.24077927088272,0.0621170768093258,
-0.956719207315372));
#27805=CARTESIAN_POINT('Ctrl Pts',(-0.246216292346804,0.0311618105631647,
-0.955720242701178));
#27806=CARTESIAN_POINT('Ctrl Pts',(-0.246044690514741,0.000148590017213961,
-0.954721278086983));
#27807=CARTESIAN_POINT('Origin',(0.,0.,-0.58));
#27808=CARTESIAN_POINT('',(-0.246140990925822,-0.000194203052083286,-0.897578721913017));
#27809=CARTESIAN_POINT('',(-0.24617270257491,-0.000203503496127644,-0.904721278086982));
#27810=CARTESIAN_POINT('',(-0.24635,-3.0169173896995E-17,-0.58));
#27811=CARTESIAN_POINT('Ctrl Pts',(-0.246140990925822,-0.000194203052083286,
-0.897578721913017));
#27812=CARTESIAN_POINT('Ctrl Pts',(-0.245730015818884,0.0551480007569202,
-0.899363101788541));
#27813=CARTESIAN_POINT('Ctrl Pts',(-0.227258101070754,0.110738834210626,
-0.901147481664065));
#27814=CARTESIAN_POINT('Ctrl Pts',(-0.192994105070856,0.15374889461325,
-0.902931861539588));
#27815=CARTESIAN_POINT('Ctrl Pts',(-0.142297419606602,0.217386174515947,
-0.905572013181517));
#27816=CARTESIAN_POINT('Ctrl Pts',(-0.0570288952207411,0.253481773718221,
-0.908212164823445));
#27817=CARTESIAN_POINT('Ctrl Pts',(0.0239494621323068,0.245584752072496,
-0.910852316465374));
#27818=CARTESIAN_POINT('Ctrl Pts',(0.104927819485355,0.237687730426771,
-0.913492468107302));
#27819=CARTESIAN_POINT('Ctrl Pts',(0.181616009805589,0.185798087933047,
-0.916132619749232));
#27820=CARTESIAN_POINT('Ctrl Pts',(0.219062602535076,0.113565062221743,
-0.91877277139116));
#27821=CARTESIAN_POINT('Ctrl Pts',(0.256509195264563,0.0413320365104399,
-0.921412923033089));
#27822=CARTESIAN_POINT('Ctrl Pts',(0.254714190403302,-0.0512443724184431,
-0.924053074675017));
#27823=CARTESIAN_POINT('Ctrl Pts',(0.214495679856809,-0.121971515156742,
-0.926693226316946));
#27824=CARTESIAN_POINT('Ctrl Pts',(0.174277169310317,-0.192698657895042,
-0.929333377958874));
#27825=CARTESIAN_POINT('Ctrl Pts',(0.0956351530785919,-0.241576534442757,
-0.931973529600803));
#27826=CARTESIAN_POINT('Ctrl Pts',(0.0144115379507457,-0.246328550438247,
-0.934613681242732));
#27827=CARTESIAN_POINT('Ctrl Pts',(-0.0668120771770993,-0.251080566433737,
-0.937253832884661));
#27828=CARTESIAN_POINT('Ctrl Pts',(-0.150617291201066,-0.211706721877003,
-0.939893984526589));
#27829=CARTESIAN_POINT('Ctrl Pts',(-0.198809016897293,-0.146152050915969,
-0.942534136168517));
#27830=CARTESIAN_POINT('Ctrl Pts',(-0.229502619061303,-0.104399883683908,
-0.944215664750017));
#27831=CARTESIAN_POINT('Ctrl Pts',(-0.245749633547702,-0.0520274817631998,
-0.945897193331517));
#27832=CARTESIAN_POINT('Ctrl Pts',(-0.246068967124758,0.000163257868156283,
-0.947578721913017));
#27833=CARTESIAN_POINT('Ctrl Pts',(-0.246044690514741,0.000148590017213961,
-0.954721278086983));
#27834=CARTESIAN_POINT('Ctrl Pts',(-0.245762767915366,-0.0508026594314752,
-0.953080091059249));
#27835=CARTESIAN_POINT('Ctrl Pts',(-0.230342715915977,-0.101910332238121,
-0.951438904031516));
#27836=CARTESIAN_POINT('Ctrl Pts',(-0.201008675250746,-0.143111693871055,
-0.949797717003782));
#27837=CARTESIAN_POINT('Ctrl Pts',(-0.153819467489548,-0.209391673377774,
-0.947157565361853));
#27838=CARTESIAN_POINT('Ctrl Pts',(-0.0706227374306924,-0.250035458329393,
-0.944517413719924));
#27839=CARTESIAN_POINT('Ctrl Pts',(0.0106637505259729,-0.246519226181408,
-0.941877262077995));
#27840=CARTESIAN_POINT('Ctrl Pts',(0.0919502384826396,-0.243002994033424,
-0.939237110436067));
#27841=CARTESIAN_POINT('Ctrl Pts',(0.171326484337116,-0.195326744785834,
-0.936596958794139));
#27842=CARTESIAN_POINT('Ctrl Pts',(0.212615948603837,-0.125219418822052,
-0.93395680715221));
#27843=CARTESIAN_POINT('Ctrl Pts',(0.253905412870557,-0.0551120928582709,
-0.931316655510282));
#27844=CARTESIAN_POINT('Ctrl Pts',(0.257108095549521,0.0374263098217014,
-0.928676503868353));
#27845=CARTESIAN_POINT('Ctrl Pts',(0.220764341110336,0.110220461552371,
-0.926036352226424));
#27846=CARTESIAN_POINT('Ctrl Pts',(0.18442058667115,0.183014613283042,-0.923396200584495));
#27847=CARTESIAN_POINT('Ctrl Pts',(0.108530395113813,0.236064514064409,
-0.920756048942567));
#27848=CARTESIAN_POINT('Ctrl Pts',(0.0276815008613437,0.245192126629843,
-0.918115897300638));
#27849=CARTESIAN_POINT('Ctrl Pts',(-0.0531673933911258,0.254319739195276,
-0.915475745658709));
#27850=CARTESIAN_POINT('Ctrl Pts',(-0.138974990338729,0.219525063544776,
-0.912835594016781));
#27851=CARTESIAN_POINT('Ctrl Pts',(-0.19063359616867,0.156666130553969,
-0.910195442374852));
#27852=CARTESIAN_POINT('Ctrl Pts',(-0.22633706242725,0.113221640385657,
-0.908370720945562));
#27853=CARTESIAN_POINT('Ctrl Pts',(-0.245728300868163,0.0563714669369404,
-0.906545999516272));
#27854=CARTESIAN_POINT('Ctrl Pts',(-0.24617270257491,-0.000203503496127644,
-0.904721278086982));
#27855=CARTESIAN_POINT('Origin',(0.,0.,-0.58));
#27856=CARTESIAN_POINT('',(-0.24674826027019,-1.7099131415399E-5,-0.847578721913017));
#27857=CARTESIAN_POINT('',(-0.246749580224057,5.88930587390795E-6,-0.854721278086983));
#27858=CARTESIAN_POINT('',(-0.24635,-3.0169173896995E-17,-0.58));
#27859=CARTESIAN_POINT('Ctrl Pts',(-0.24674826027019,-1.7099131415399E-5,
-0.847578721913017));
#27860=CARTESIAN_POINT('Ctrl Pts',(-0.246667412551575,0.0804217509967416,
-0.850188858603636));
#27861=CARTESIAN_POINT('Ctrl Pts',(-0.203606490563192,0.160934891961365,
-0.852798995294255));
#27862=CARTESIAN_POINT('Ctrl Pts',(-0.136624724734367,0.205472946584612,
-0.855409131984873));
#27863=CARTESIAN_POINT('Ctrl Pts',(-0.0688727101874428,0.25052316118238,
-0.858049283626802));
#27864=CARTESIAN_POINT('Ctrl Pts',(0.0233534610933846,0.258766149935299,
-0.86068943526873));
#27865=CARTESIAN_POINT('Ctrl Pts',(0.0980207641052817,0.226445086038806,
-0.863329586910659));
#27866=CARTESIAN_POINT('Ctrl Pts',(0.172688067117179,0.194124022142313,
-0.865969738552587));
#27867=CARTESIAN_POINT('Ctrl Pts',(0.229796501860146,0.121238905596409,
-0.868609890194516));
#27868=CARTESIAN_POINT('Ctrl Pts',(0.243318312523803,0.0410078770173896,
-0.871250041836445));
#27869=CARTESIAN_POINT('Ctrl Pts',(0.25684012318746,-0.0392231515616299,
-0.873890193478373));
#27870=CARTESIAN_POINT('Ctrl Pts',(0.226775309771808,-0.126800092173765,
-0.876530345120302));
#27871=CARTESIAN_POINT('Ctrl Pts',(0.166826219847552,-0.181808854455111,
-0.87917049676223));
#27872=CARTESIAN_POINT('Ctrl Pts',(0.106877129923296,-0.236817616736456,
-0.881810648404159));
#27873=CARTESIAN_POINT('Ctrl Pts',(0.0170437634904362,-0.259258200687012,
-0.884450800046088));
#27874=CARTESIAN_POINT('Ctrl Pts',(-0.061731399838991,-0.238903079638643,
-0.887090951688017));
#27875=CARTESIAN_POINT('Ctrl Pts',(-0.140506563168418,-0.218547958590274,
-0.889731103329945));
#27876=CARTESIAN_POINT('Ctrl Pts',(-0.208223523394413,-0.15539713254298,
-0.892371254971873));
#27877=CARTESIAN_POINT('Ctrl Pts',(-0.234019580236086,-0.0782322392177732,
-0.895011406613802));
#27878=CARTESIAN_POINT('Ctrl Pts',(-0.242381045834917,-0.0532202149019548,
-0.895867178380207));
#27879=CARTESIAN_POINT('Ctrl Pts',(-0.24633809071272,-0.0267358022709602,
-0.896722950146612));
#27880=CARTESIAN_POINT('Ctrl Pts',(-0.246140990925822,-0.000194203052083286,
-0.897578721913017));
#27881=CARTESIAN_POINT('Ctrl Pts',(-0.24617270257491,-0.000203503496127644,
-0.904721278086982));
#27882=CARTESIAN_POINT('Ctrl Pts',(-0.24637129649309,-0.0254856859869767,
-0.903905847874344));
#27883=CARTESIAN_POINT('Ctrl Pts',(-0.242786186315468,-0.0507129101334804,
-0.903090417661705));
#27884=CARTESIAN_POINT('Ctrl Pts',(-0.235182253523972,-0.0746642623906653,
-0.902274987449066));
#27885=CARTESIAN_POINT('Ctrl Pts',(-0.210562690337051,-0.152212532013379,
-0.899634835807138));
#27886=CARTESIAN_POINT('Ctrl Pts',(-0.143813949250927,-0.216385880927691,
-0.896994684165209));
#27887=CARTESIAN_POINT('Ctrl Pts',(-0.0653574547268311,-0.237936646111214,
-0.894354532523281));
#27888=CARTESIAN_POINT('Ctrl Pts',(0.0130990397972646,-0.259487411294737,
-0.891714380881352));
#27889=CARTESIAN_POINT('Ctrl Pts',(0.103263287759333,-0.238415592747473,
-0.889074229239423));
#27890=CARTESIAN_POINT('Ctrl Pts',(0.164042006891183,-0.184324888243821,
-0.886434077597494));
#27891=CARTESIAN_POINT('Ctrl Pts',(0.224820726023033,-0.130234183740168,
-0.883793925955566));
#27892=CARTESIAN_POINT('Ctrl Pts',(0.256213916324662,-0.0431245932801274,
-0.881153774313637));
#27893=CARTESIAN_POINT('Ctrl Pts',(0.243913808813169,0.0373027924054035,
-0.878513622671709));
#27894=CARTESIAN_POINT('Ctrl Pts',(0.231613701301676,0.117730178090933,
-0.87587347102978));
#27895=CARTESIAN_POINT('Ctrl Pts',(0.175620295977063,0.191475359001952,
-0.873233319387852));
#27896=CARTESIAN_POINT('Ctrl Pts',(0.101453162537552,0.224928211352256,
-0.870593167745923));
#27897=CARTESIAN_POINT('Ctrl Pts',(0.0272860290980399,0.258381063702561,
-0.867953016103994));
#27898=CARTESIAN_POINT('Ctrl Pts',(-0.0650548324563724,0.251541587492149,
-0.865312864462065));
#27899=CARTESIAN_POINT('Ctrl Pts',(-0.133484125852437,0.207526944266042,
-0.862672712820137));
#27900=CARTESIAN_POINT('Ctrl Pts',(-0.202181071340161,0.16334014360942,
-0.860022234575752));
#27901=CARTESIAN_POINT('Ctrl Pts',(-0.246778412616135,0.0816867933466605,
-0.857371756331367));
#27902=CARTESIAN_POINT('Ctrl Pts',(-0.246749580224057,5.88930587390795E-6,
-0.854721278086983));
#27903=CARTESIAN_POINT('Origin',(0.,0.,-0.58));
#27904=CARTESIAN_POINT('',(-0.246188793287857,0.000207412629416426,-0.797578721913017));
#27905=CARTESIAN_POINT('',(-0.246156246887236,0.000198954902853581,-0.804721278086982));
#27906=CARTESIAN_POINT('',(-0.24635,-3.0169173896995E-17,-0.58));
#27907=CARTESIAN_POINT('Ctrl Pts',(-0.246188793287857,0.000207412629416426,
-0.797578721913017));
#27908=CARTESIAN_POINT('Ctrl Pts',(-0.246387252386039,0.0248750860659389,
-0.798374463776802));
#27909=CARTESIAN_POINT('Ctrl Pts',(-0.242976611149663,0.049489136932403,
-0.799170205640587));
#27910=CARTESIAN_POINT('Ctrl Pts',(-0.235729958539167,0.0729166224809383,
-0.799965947504372));
#27911=CARTESIAN_POINT('Ctrl Pts',(-0.211686656736383,0.150645490663177,
-0.802606099146301));
#27912=CARTESIAN_POINT('Ctrl Pts',(-0.145416064350721,0.21531250016226,
-0.805246250788229));
#27913=CARTESIAN_POINT('Ctrl Pts',(-0.0671216846612779,0.237444997073294,
-0.807886402430158));
#27914=CARTESIAN_POINT('Ctrl Pts',(0.0111726950281651,0.259577493984328,
-0.810526554072086));
#27915=CARTESIAN_POINT('Ctrl Pts',(0.101490862021389,0.239175478307313,
-0.813166705714014));
#27916=CARTESIAN_POINT('Ctrl Pts',(0.16266938387061,0.185537378277427,-0.815806857355943));
#27917=CARTESIAN_POINT('Ctrl Pts',(0.223847905719831,0.131899278247541,
-0.818447008997872));
#27918=CARTESIAN_POINT('Ctrl Pts',(0.255886782425048,0.0450250938647844,
-0.821087160639801));
#27919=CARTESIAN_POINT('Ctrl Pts',(0.244183966791736,-0.0354913728778911,
-0.82372731228173));
#27920=CARTESIAN_POINT('Ctrl Pts',(0.232481151158423,-0.116007839620565,
-0.826367463923659));
#27921=CARTESIAN_POINT('Ctrl Pts',(0.177036643186582,-0.190166588723159,
-0.829007615565587));
#27922=CARTESIAN_POINT('Ctrl Pts',(0.103119846967095,-0.224169008447617,
-0.831647767207515));
#27923=CARTESIAN_POINT('Ctrl Pts',(0.0292030507476063,-0.258171428172075,
-0.834287918849444));
#27924=CARTESIAN_POINT('Ctrl Pts',(-0.0631860337195292,-0.252017518518398,
-0.836928070491373));
#27925=CARTESIAN_POINT('Ctrl Pts',(-0.131940132073209,-0.208511987030504,
-0.839568222133302));
#27926=CARTESIAN_POINT('Ctrl Pts',(-0.200694230426889,-0.16500645554261,
-0.84220837377523));
#27927=CARTESIAN_POINT('Ctrl Pts',(-0.245813342667112,-0.0841493022204997,
-0.844848525417158));
#27928=CARTESIAN_POINT('Ctrl Pts',(-0.246733969880713,-0.00279200533813568,
-0.847488677059087));
#27929=CARTESIAN_POINT('Ctrl Pts',(-0.246744436166267,-0.00186708297160882,
-0.847518692010397));
#27930=CARTESIAN_POINT('Ctrl Pts',(-0.246749189968755,-0.000942095963463235,
-0.847548706961707));
#27931=CARTESIAN_POINT('Ctrl Pts',(-0.24674826027019,-1.7099131415399E-5,
-0.847578721913017));
#27932=CARTESIAN_POINT('Ctrl Pts',(-0.246749580224057,5.88930587390795E-6,
-0.854721278086983));
#27933=CARTESIAN_POINT('Ctrl Pts',(-0.246720972501359,-0.0810385362230983,
-0.85209145304751));
#27934=CARTESIAN_POINT('Ctrl Pts',(-0.202914101569483,-0.162109483810441,
-0.849461628008038));
#27935=CARTESIAN_POINT('Ctrl Pts',(-0.13509588376053,-0.206481346958881,
-0.846831802968566));
#27936=CARTESIAN_POINT('Ctrl Pts',(-0.0670113623898996,-0.251027446257671,
-0.844191651326637));
#27937=CARTESIAN_POINT('Ctrl Pts',(0.0252734480549719,-0.258585680747039,
-0.841551499684708));
#27938=CARTESIAN_POINT('Ctrl Pts',(0.0996987971698373,-0.225711307412542,
-0.838911348042779));
#27939=CARTESIAN_POINT('Ctrl Pts',(0.174124146284703,-0.192836934078045,
-0.83627119640085));
#27940=CARTESIAN_POINT('Ctrl Pts',(0.230690034069562,-0.119529952919682,
-0.833631044758922));
#27941=CARTESIAN_POINT('Ctrl Pts',(0.24361597606379,-0.0392007736846921,
-0.830990893116994));
#27942=CARTESIAN_POINT('Ctrl Pts',(0.256541918058019,0.0411284055502995,
-0.828350741475065));
#27943=CARTESIAN_POINT('Ctrl Pts',(0.225827914261615,0.128479782861919,
-0.825710589833136));
#27944=CARTESIAN_POINT('Ctrl Pts',(0.165472187430463,0.183042070677671,
-0.823070438191208));
#27945=CARTESIAN_POINT('Ctrl Pts',(0.105116460599312,0.237604358493422,
-0.820430286549279));
#27946=CARTESIAN_POINT('Ctrl Pts',(0.0151190107334124,0.259377556813307,
-0.81779013490735));
#27947=CARTESIAN_POINT('Ctrl Pts',(-0.063502899844963,0.238438306826467,
-0.815149983265422));
#27948=CARTESIAN_POINT('Ctrl Pts',(-0.142124810423339,0.217499056839627,
-0.812509831623493));
#27949=CARTESIAN_POINT('Ctrl Pts',(-0.209371181714192,0.153847358546061,
-0.809869679981565));
#27950=CARTESIAN_POINT('Ctrl Pts',(-0.234593789178183,0.0764931273384339,
-0.807229528339636));
#27951=CARTESIAN_POINT('Ctrl Pts',(-0.242581286378397,0.0519965836691203,
-0.806393444922085));
#27952=CARTESIAN_POINT('Ctrl Pts',(-0.246354377081631,0.0261258640936213,
-0.805557361504533));
#27953=CARTESIAN_POINT('Ctrl Pts',(-0.246156246887236,0.000198954902853581,
-0.804721278086982));
#27954=CARTESIAN_POINT('Origin',(0.,0.,-0.58));
#27955=CARTESIAN_POINT('',(-0.246033746957446,-0.000140975359651019,-0.747578721913017));
#27956=CARTESIAN_POINT('',(-0.246056814395214,-0.000156261806827737,-0.754721278086983));
#27957=CARTESIAN_POINT('',(-0.24635,-3.0169173896995E-17,-0.58));
#27958=CARTESIAN_POINT('Ctrl Pts',(-0.246033746957446,-0.000140975359651019,
-0.747578721913017));
#27959=CARTESIAN_POINT('Ctrl Pts',(-0.245770202673151,0.0502046633637533,
-0.749200220591897));
#27960=CARTESIAN_POINT('Ctrl Pts',(-0.23074455683355,0.100694729418671,
-0.750821719270777));
#27961=CARTESIAN_POINT('Ctrl Pts',(-0.202065355776875,0.141615815436235,
-0.752443217949657));
#27962=CARTESIAN_POINT('Ctrl Pts',(-0.155369394352292,0.208244221518818,
-0.755083369591585));
#27963=CARTESIAN_POINT('Ctrl Pts',(-0.0724766230355756,0.249504395974772,
-0.757723521233513));
#27964=CARTESIAN_POINT('Ctrl Pts',(0.00883372608632075,0.246591590429067,
-0.760363672875442));
#27965=CARTESIAN_POINT('Ctrl Pts',(0.0901440752082165,0.243678784883362,
-0.763003824517371));
#27966=CARTESIAN_POINT('Ctrl Pts',(0.169872002135292,0.196592999335999,
-0.765643976159301));
#27967=CARTESIAN_POINT('Ctrl Pts',(0.211680685123689,0.126794064263554,
-0.768284127801229));
#27968=CARTESIAN_POINT('Ctrl Pts',(0.253489368112086,0.056995129191111,
-0.770924279443158));
#27969=CARTESIAN_POINT('Ctrl Pts',(0.257378807161808,-0.0355169554064133,
-0.773564431085085));
#27970=CARTESIAN_POINT('Ctrl Pts',(0.221576350469646,-0.108578856594908,
-0.776204582727014));
#27971=CARTESIAN_POINT('Ctrl Pts',(0.185773893777484,-0.181640757783402,
-0.778844734368942));
#27972=CARTESIAN_POINT('Ctrl Pts',(0.110279541343437,-0.235252475562867,
-0.781484886010872));
#27973=CARTESIAN_POINT('Ctrl Pts',(0.0295006198445558,-0.244979918800893,
-0.7841250376528));
#27974=CARTESIAN_POINT('Ctrl Pts',(-0.0512783016543263,-0.254707362038918,
-0.786765189294729));
#27975=CARTESIAN_POINT('Ctrl Pts',(-0.137341792218043,-0.220550530735504,
-0.789405340936657));
#27976=CARTESIAN_POINT('Ctrl Pts',(-0.189465531889949,-0.1580767516511,
-0.792045492578586));
#27977=CARTESIAN_POINT('Ctrl Pts',(-0.225879173287477,-0.114432573342958,
-0.79388990235673));
#27978=CARTESIAN_POINT('Ctrl Pts',(-0.245728794992044,-0.0569685387198996,
-0.795734312134873));
#27979=CARTESIAN_POINT('Ctrl Pts',(-0.246188793287857,0.000207412629416426,
-0.797578721913017));
#27980=CARTESIAN_POINT('Ctrl Pts',(-0.246156246887236,0.000198954902853581,
-0.804721278086982));
#27981=CARTESIAN_POINT('Ctrl Pts',(-0.24572872927297,-0.055745119630262,
-0.802917209862605));
#27982=CARTESIAN_POINT('Ctrl Pts',(-0.226811474403897,-0.111950809230771,
-0.801113141638227));
#27983=CARTESIAN_POINT('Ctrl Pts',(-0.191847619700623,-0.15517710934992,
-0.79930907341385));
#27984=CARTESIAN_POINT('Ctrl Pts',(-0.140679999121939,-0.218436350708962,
-0.796668921771921));
#27985=CARTESIAN_POINT('Ctrl Pts',(-0.0551459143274415,-0.253898069305357,
-0.794028770129993));
#27986=CARTESIAN_POINT('Ctrl Pts',(0.0257715968441432,-0.245400222589742,
-0.791388618488064));
#27987=CARTESIAN_POINT('Ctrl Pts',(0.106689108015727,-0.236902375874126,
-0.788748466846136));
#27988=CARTESIAN_POINT('Ctrl Pts',(0.182990045564397,-0.184444963846501,
-0.786108315204207));
#27989=CARTESIAN_POINT('Ctrl Pts',(0.219899473361048,-0.111935990934666,
-0.783468163562278));
#27990=CARTESIAN_POINT('Ctrl Pts',(0.256808901157699,-0.0394270180228303,
-0.780828011920349));
#27991=CARTESIAN_POINT('Ctrl Pts',(0.25432681920233,0.0531335157732174,
-0.778187860278422));
#27992=CARTESIAN_POINT('Ctrl Pts',(0.213584461844586,0.123560196299417,
-0.775547708636493));
#27993=CARTESIAN_POINT('Ctrl Pts',(0.172842104486842,0.193986876825616,
-0.772907556994564));
#27994=CARTESIAN_POINT('Ctrl Pts',(0.0938394717267237,0.242279704081969,
-0.770267405352635));
#27995=CARTESIAN_POINT('Ctrl Pts',(0.0125828250405317,0.24642872593306,
-0.767627253710706));
#27996=CARTESIAN_POINT('Ctrl Pts',(-0.0686738216456602,0.25057774778415,
-0.764987102068778));
#27997=CARTESIAN_POINT('Ctrl Pts',(-0.152184482257925,0.210582964229978,
-0.762346950426849));
#27998=CARTESIAN_POINT('Ctrl Pts',(-0.199888315315273,0.144672408742696,
-0.759706798784921));
#27999=CARTESIAN_POINT('Ctrl Pts',(-0.229915434881869,0.103185089936717,
-0.758044958552275));
#28000=CARTESIAN_POINT('Ctrl Pts',(-0.245755682841279,0.0514297928114553,
-0.756383118319629));
#28001=CARTESIAN_POINT('Ctrl Pts',(-0.246056814395214,-0.000156261806827737,
-0.754721278086983));
#28002=CARTESIAN_POINT('Origin',(0.,0.,-0.58));
#28003=CARTESIAN_POINT('',(-0.246694142079541,-0.000104913238225313,-0.697578721913017));
#28004=CARTESIAN_POINT('',(-0.24671395673833,-8.44291920866902E-5,-0.704721278086983));
#28005=CARTESIAN_POINT('',(-0.24635,-3.0169173896995E-17,-0.58));
#28006=CARTESIAN_POINT('Ctrl Pts',(-0.246694142079541,-0.000104913238225313,
-0.697578721913017));
#28007=CARTESIAN_POINT('Ctrl Pts',(-0.246288608374016,0.0753584670996666,
-0.700025977406992));
#28008=CARTESIAN_POINT('Ctrl Pts',(-0.209097267103025,0.151167615813192,
-0.702473232900967));
#28009=CARTESIAN_POINT('Ctrl Pts',(-0.148976321364386,0.196701557847517,
-0.704920488394942));
#28010=CARTESIAN_POINT('Ctrl Pts',(-0.0841165574382396,0.24582454975473,
-0.707560640036871));
#28011=CARTESIAN_POINT('Ctrl Pts',(0.00742995623837037,0.259711571262569,
-0.710200791678799));
#28012=CARTESIAN_POINT('Ctrl Pts',(0.0839399555978737,0.232033469657142,
-0.712840943320728));
#28013=CARTESIAN_POINT('Ctrl Pts',(0.160449954957377,0.204355368051715,
-0.715481094962656));
#28014=CARTESIAN_POINT('Ctrl Pts',(0.221923439999773,0.135112143333024,
-0.718121246604584));
#28015=CARTESIAN_POINT('Ctrl Pts',(0.240343238398454,0.0558621065038622,
-0.720761398246513));
#28016=CARTESIAN_POINT('Ctrl Pts',(0.258763036797135,-0.0233879303253011,
-0.723401549888442));
#28017=CARTESIAN_POINT('Ctrl Pts',(0.234129148552099,-0.112644779264936,
-0.726041701530371));
#28018=CARTESIAN_POINT('Ctrl Pts',(0.177668721295525,-0.171228714473122,
-0.728681853172299));
#28019=CARTESIAN_POINT('Ctrl Pts',(0.121208294038953,-0.229812649681307,
-0.731322004814228));
#28020=CARTESIAN_POINT('Ctrl Pts',(0.0329213277708455,-0.257723671158046,
-0.733962156456156));
#28021=CARTESIAN_POINT('Ctrl Pts',(-0.0469544856580573,-0.242241044134746,
-0.736602308098085));
#28022=CARTESIAN_POINT('Ctrl Pts',(-0.12683029908696,-0.226758417111446,
-0.739242459740013));
#28023=CARTESIAN_POINT('Ctrl Pts',(-0.198294959676658,-0.167882141588106,
-0.741882611381942));
#28024=CARTESIAN_POINT('Ctrl Pts',(-0.228777714205282,-0.0924456849718314,
-0.744522763023871));
#28025=CARTESIAN_POINT('Ctrl Pts',(-0.240538912967255,-0.0633399439099515,
-0.74554141598692));
#28026=CARTESIAN_POINT('Ctrl Pts',(-0.246199309945309,-0.0317689592304798,
-0.746560068949969));
#28027=CARTESIAN_POINT('Ctrl Pts',(-0.246033746957446,-0.000140975359651019,
-0.747578721913017));
#28028=CARTESIAN_POINT('Ctrl Pts',(-0.246056814395214,-0.000156261806827737,
-0.754721278086983));
#28029=CARTESIAN_POINT('Ctrl Pts',(-0.24623408801582,-0.0305245395759718,
-0.7537429666777));
#28030=CARTESIAN_POINT('Ctrl Pts',(-0.241026159380574,-0.0608341650313951,
-0.752764655268417));
#28031=CARTESIAN_POINT('Ctrl Pts',(-0.230157149346615,-0.0889557814626542,
-0.751786343859135));
#28032=CARTESIAN_POINT('Ctrl Pts',(-0.20082514481818,-0.164847088760323,
-0.749146192217206));
#28033=CARTESIAN_POINT('Ctrl Pts',(-0.130264130258884,-0.224803375935269,
-0.746506040575278));
#28034=CARTESIAN_POINT('Ctrl Pts',(-0.0506330129290607,-0.241498949175182,
-0.743865888933349));
#28035=CARTESIAN_POINT('Ctrl Pts',(0.028998104400764,-0.258194522415096,
-0.741225737291421));
#28036=CARTESIAN_POINT('Ctrl Pts',(0.117699324501114,-0.231629381719977,
-0.738585585649492));
#28037=CARTESIAN_POINT('Ctrl Pts',(0.175044155081566,-0.17391086286593,
-0.735945434007563));
#28038=CARTESIAN_POINT('Ctrl Pts',(0.232388985662017,-0.116192344011885,
-0.733305282365635));
#28039=CARTESIAN_POINT('Ctrl Pts',(0.258377426722569,-0.0273204469989132,
-0.730665130723706));
#28040=CARTESIAN_POINT('Ctrl Pts',(0.24116497927002,0.0522005481262653,
-0.728024979081777));
#28041=CARTESIAN_POINT('Ctrl Pts',(0.22395253181747,0.131721543251444,-0.725384827439849));
#28042=CARTESIAN_POINT('Ctrl Pts',(0.163539195851817,0.201891636488831,
-0.72274467579792));
#28043=CARTESIAN_POINT('Ctrl Pts',(0.0874589698670081,0.230730086986491,
-0.720104524155991));
#28044=CARTESIAN_POINT('Ctrl Pts',(0.0113787438821998,0.25956853748415,
-0.717464372514063));
#28045=CARTESIAN_POINT('Ctrl Pts',(-0.0803683721217641,0.247075345242084,
-0.714824220872134));
#28046=CARTESIAN_POINT('Ctrl Pts',(-0.145967687505829,0.198944410967467,
-0.712184069230205));
#28047=CARTESIAN_POINT('Ctrl Pts',(-0.207776509655161,0.153594602984812,
-0.709696472182465));
#28048=CARTESIAN_POINT('Ctrl Pts',(-0.246371999630066,0.0766065415301417,
-0.707208875134724));
#28049=CARTESIAN_POINT('Ctrl Pts',(-0.24671395673833,-8.44291920866902E-5,
-0.704721278086983));
#28050=CARTESIAN_POINT('Origin',(0.,0.,-0.58));
#28051=CARTESIAN_POINT('',(-0.246332988773408,0.00022261242931975,-0.647578721913017));
#28052=CARTESIAN_POINT('',(-0.246295889561636,0.000221807446104811,-0.654721278086982));
#28053=CARTESIAN_POINT('',(-0.24635,-3.0169173896995E-17,-0.58));
#28054=CARTESIAN_POINT('Ctrl Pts',(-0.246332988773408,0.00022261242931975,
-0.647578721913017));
#28055=CARTESIAN_POINT('Ctrl Pts',(-0.246510645363659,0.0198118416510094,
-0.648211582580158));
#28056=CARTESIAN_POINT('Ctrl Pts',(-0.244369383537724,0.0393627020095402,
-0.648844443247299));
#28057=CARTESIAN_POINT('Ctrl Pts',(-0.23976029777941,0.0583133500635451,
-0.64947730391444));
#28058=CARTESIAN_POINT('Ctrl Pts',(-0.220532233903086,0.137371169854126,
-0.652117455556369));
#28059=CARTESIAN_POINT('Ctrl Pts',(-0.158354907967284,0.2059830760525,-0.654757607198297));
#28060=CARTESIAN_POINT('Ctrl Pts',(-0.0815662750163546,0.232878487557055,
-0.657397758840226));
#28061=CARTESIAN_POINT('Ctrl Pts',(-0.00477764206542863,0.259773899061609,
-0.660037910482155));
#28062=CARTESIAN_POINT('Ctrl Pts',(0.0866222979006217,0.244952815872347,
-0.662678062124084));
#28063=CARTESIAN_POINT('Ctrl Pts',(0.15097708328857,0.195170098910107,-0.665318213766013));
#28064=CARTESIAN_POINT('Ctrl Pts',(0.215331868676519,0.145387381947866,
-0.667958365407941));
#28065=CARTESIAN_POINT('Ctrl Pts',(0.252641499486365,0.0606430312126439,
-0.67059851704987));
#28066=CARTESIAN_POINT('Ctrl Pts',(0.245901728193816,-0.0204398448673013,
-0.673238668691798));
#28067=CARTESIAN_POINT('Ctrl Pts',(0.239161956901268,-0.101522720947246,
-0.675878820333726));
#28068=CARTESIAN_POINT('Ctrl Pts',(0.188372783506328,-0.178944122371914,
-0.678518971975655));
#28069=CARTESIAN_POINT('Ctrl Pts',(0.116681895542094,-0.217418450090163,
-0.681159123617584));
#28070=CARTESIAN_POINT('Ctrl Pts',(0.0449910075778601,-0.255892777808412,
-0.683799275259513));
#28071=CARTESIAN_POINT('Ctrl Pts',(-0.0476015949556688,-0.255420031820241,
-0.686439426901442));
#28072=CARTESIAN_POINT('Ctrl Pts',(-0.118895882247883,-0.216215670966289,
-0.68907957854337));
#28073=CARTESIAN_POINT('Ctrl Pts',(-0.190190169540097,-0.177011310112337,
-0.691719730185299));
#28074=CARTESIAN_POINT('Ctrl Pts',(-0.240186141590997,-0.0990753343926033,
-0.694359881827227));
#28075=CARTESIAN_POINT('Ctrl Pts',(-0.246097620528605,-0.0179278653794423,
-0.697000033469156));
#28076=CARTESIAN_POINT('Ctrl Pts',(-0.246529528112119,-0.0119990263157112,
-0.69719292961711));
#28077=CARTESIAN_POINT('Ctrl Pts',(-0.246726106821209,-0.00605304387460213,
-0.697385825765063));
#28078=CARTESIAN_POINT('Ctrl Pts',(-0.246694142079541,-0.000104913238225313,
-0.697578721913017));
#28079=CARTESIAN_POINT('Ctrl Pts',(-0.24671395673833,-8.44291920866902E-5,
-0.704721278086983));
#28080=CARTESIAN_POINT('Ctrl Pts',(-0.246734927629869,-0.00478758637222922,
-0.704568723492795));
#28081=CARTESIAN_POINT('Ctrl Pts',(-0.246612031230182,-0.00948962622710204,
-0.704416168898608));
#28082=CARTESIAN_POINT('Ctrl Pts',(-0.246341798658231,-0.0141831831694928,
-0.70426361430442));
#28083=CARTESIAN_POINT('Ctrl Pts',(-0.241665079662402,-0.0954111667246658,
-0.701623462662492));
#28084=CARTESIAN_POINT('Ctrl Pts',(-0.19286012690658,-0.174098457527845,
-0.698983311020563));
#28085=CARTESIAN_POINT('Ctrl Pts',(-0.122170298983642,-0.214382514439119,
-0.696343159378634));
#28086=CARTESIAN_POINT('Ctrl Pts',(-0.0514804710607036,-0.254666571350394,
-0.693703007736705));
#28087=CARTESIAN_POINT('Ctrl Pts',(0.0410942320293508,-0.256547394369764,
-0.691062856094777));
#28088=CARTESIAN_POINT('Ctrl Pts',(0.113361938331161,-0.219167779084413,
-0.688422704452848));
#28089=CARTESIAN_POINT('Ctrl Pts',(0.185629644632971,-0.181788163799061,
-0.68578255281092));
#28090=CARTESIAN_POINT('Ctrl Pts',(0.237590354146535,-0.105148110208987,
-0.683142401168991));
#28091=CARTESIAN_POINT('Ctrl Pts',(0.245562439717473,-0.0241771100629151,
-0.680502249527062));
#28092=CARTESIAN_POINT('Ctrl Pts',(0.25353452528841,0.0567938900831571,
-0.677862097885134));
#28093=CARTESIAN_POINT('Ctrl Pts',(0.217517986916721,0.142095836785229,
-0.675221946243205));
#28094=CARTESIAN_POINT('Ctrl Pts',(0.153927731964037,0.192851491524954,
-0.672581794601276));
#28095=CARTESIAN_POINT('Ctrl Pts',(0.0903374770113528,0.243607146264678,
-0.669941642959348));
#28096=CARTESIAN_POINT('Ctrl Pts',(-0.000826494522324708,0.259816509042058,
-0.667301491317419));
#28097=CARTESIAN_POINT('Ctrl Pts',(-0.0780152660809326,0.234091996252142,
-0.66466133967549));
#28098=CARTESIAN_POINT('Ctrl Pts',(-0.15520403763954,0.208367483462227,
-0.662021188033562));
#28099=CARTESIAN_POINT('Ctrl Pts',(-0.218417609223077,0.140709095105016,
-0.659381036391633));
#28100=CARTESIAN_POINT('Ctrl Pts',(-0.23884574618786,0.0619528367305004,
-0.656740884749705));
#28101=CARTESIAN_POINT('Ctrl Pts',(-0.244054639099651,0.0418710780897904,
-0.656067682528797));
#28102=CARTESIAN_POINT('Ctrl Pts',(-0.246481710354252,0.0210677585852516,
-0.65539448030789));
#28103=CARTESIAN_POINT('Ctrl Pts',(-0.246295889561636,0.000221807446104811,
-0.654721278086982));
#28104=CARTESIAN_POINT('Origin',(0.,0.,-0.58));
#28105=CARTESIAN_POINT('',(-0.245967927871332,-6.88792904169344E-5,-0.597578721913017));
#28106=CARTESIAN_POINT('',(-0.245979910166711,-8.79836153418138E-5,-0.604721278086982));
#28107=CARTESIAN_POINT('',(-0.24635,-3.0169173896995E-17,-0.58));
#28108=CARTESIAN_POINT('Ctrl Pts',(-0.245967927871332,-6.88792904169344E-5,
-0.597578721913017));
#28109=CARTESIAN_POINT('Ctrl Pts',(-0.245853915264038,0.0452498307293128,
-0.599037339395253));
#28110=CARTESIAN_POINT('Ctrl Pts',(-0.233865752530936,0.0906246440450581,
-0.600495956877489));
#28111=CARTESIAN_POINT('Ctrl Pts',(-0.210374949312293,0.128948935198221,
-0.601954574359725));
#28112=CARTESIAN_POINT('Ctrl Pts',(-0.167855725839909,0.198317320978612,
-0.604594726001654));
#28113=CARTESIAN_POINT('Ctrl Pts',(-0.0876511603303029,0.244586546216524,
-0.607234877643583));
#28114=CARTESIAN_POINT('Ctrl Pts',(-0.00631530745783936,0.246668936184956,
-0.609875029285512));
#28115=CARTESIAN_POINT('Ctrl Pts',(0.0750205454146241,0.248751326153387,
-0.61251518092744));
#28116=CARTESIAN_POINT('Ctrl Pts',(0.157487685649946,0.206646880852338,
-0.615155332569368));
#28117=CARTESIAN_POINT('Ctrl Pts',(0.203500866899034,0.139545133767704,
-0.617795484211297));
#28118=CARTESIAN_POINT('Ctrl Pts',(0.249514048148123,0.0724433866830698,
-0.620435635853225));
#28119=CARTESIAN_POINT('Ctrl Pts',(0.259073270410978,-0.0196556621851494,
-0.623075787495155));
#28120=CARTESIAN_POINT('Ctrl Pts',(0.227821819939192,-0.0947769251795984,
-0.625715939137083));
#28121=CARTESIAN_POINT('Ctrl Pts',(0.196570369467406,-0.169898188174047,
-0.628356090779012));
#28122=CARTESIAN_POINT('Ctrl Pts',(0.124508246260982,-0.228041665294725,
-0.63099624242094));
#28123=CARTESIAN_POINT('Ctrl Pts',(0.0444785032671047,-0.242707869534597,
-0.633636394062869));
#28124=CARTESIAN_POINT('Ctrl Pts',(-0.0355512397267712,-0.257374073774469,
-0.636276545704797));
#28125=CARTESIAN_POINT('Ctrl Pts',(-0.123548602508098,-0.228563005133535,
-0.638916697346726));
#28126=CARTESIAN_POINT('Ctrl Pts',(-0.179407882990338,-0.169405604121676,
-0.641556848988655));
#28127=CARTESIAN_POINT('Ctrl Pts',(-0.22187734867914,-0.12442859777963,
-0.643564139963442));
#28128=CARTESIAN_POINT('Ctrl Pts',(-0.245769502229312,-0.0619099944166167,
-0.64557143093823));
#28129=CARTESIAN_POINT('Ctrl Pts',(-0.246332988773408,0.00022261242931975,
-0.647578721913017));
#28130=CARTESIAN_POINT('Ctrl Pts',(-0.246295889561636,0.000221807446104811,
-0.654721278086982));
#28131=CARTESIAN_POINT('Ctrl Pts',(-0.245752961910631,-0.0606854953677682,
-0.652754328665961));
#28132=CARTESIAN_POINT('Ctrl Pts',(-0.222904287268899,-0.121956736085764,
-0.65078737924494));
#28133=CARTESIAN_POINT('Ctrl Pts',(-0.181963421308779,-0.166657606356852,
-0.648820429823918));
#28134=CARTESIAN_POINT('Ctrl Pts',(-0.127010257118888,-0.226657662677861,
-0.64618027818199));
#28135=CARTESIAN_POINT('Ctrl Pts',(-0.0394612263930818,-0.256803646928059,
-0.643540126540062));
#28136=CARTESIAN_POINT('Ctrl Pts',(0.0407823007221384,-0.243356217095025,
-0.640899974898133));
#28137=CARTESIAN_POINT('Ctrl Pts',(0.121025827837359,-0.229908787261991,
-0.638259823256204));
#28138=CARTESIAN_POINT('Ctrl Pts',(0.193963851341991,-0.17286794334572,
-0.635619671614275));
#28139=CARTESIAN_POINT('Ctrl Pts',(0.22635411772979,-0.0982306359429682,
-0.632979519972347));
#28140=CARTESIAN_POINT('Ctrl Pts',(0.258744384117589,-0.0235933285402166,
-0.630339368330418));
#28141=CARTESIAN_POINT('Ctrl Pts',(0.250586893388558,0.0686404423490178,
-0.62769921668849));
#28142=CARTESIAN_POINT('Ctrl Pts',(0.205599505744543,0.136434188122301,
-0.625059065046561));
#28143=CARTESIAN_POINT('Ctrl Pts',(0.160612118100527,0.204227933895586,
-0.622418913404633));
#28144=CARTESIAN_POINT('Ctrl Pts',(0.0787948335415277,0.247581654552918,
-0.619778761762704));
#28145=CARTESIAN_POINT('Ctrl Pts',(-0.00256327998383143,0.246736446530942,
-0.617138610120775));
#28146=CARTESIAN_POINT('Ctrl Pts',(-0.0839213935091894,0.245891238508966,
-0.614498458478847));
#28147=CARTESIAN_POINT('Ctrl Pts',(-0.164820336000906,0.200847101807682,
-0.611858306836918));
#28148=CARTESIAN_POINT('Ctrl Pts',(-0.208389583341672,0.132133364468162,
-0.609218155194989));
#28149=CARTESIAN_POINT('Ctrl Pts',(-0.233126237083863,0.0931208032778008,
-0.607719196158987));
#28150=CARTESIAN_POINT('Ctrl Pts',(-0.245829826783415,0.0464784497949531,
-0.606220237122985));
#28151=CARTESIAN_POINT('Ctrl Pts',(-0.245979910166711,-8.79836153418138E-5,
-0.604721278086982));
#28152=CARTESIAN_POINT('Origin',(0.,0.,-0.58));
#28153=CARTESIAN_POINT('',(-0.246582462449767,-0.000173722512632146,-0.547578721913017));
#28154=CARTESIAN_POINT('',(-0.246614023415026,-0.000159075665185677,-0.554721278086982));
#28155=CARTESIAN_POINT('',(-0.24635,-3.0169173896995E-17,-0.58));
#28156=CARTESIAN_POINT('Ctrl Pts',(-0.246582462449767,-0.000173722512632146,
-0.547578721913017));
#28157=CARTESIAN_POINT('Ctrl Pts',(-0.246017207900454,0.0703510165357913,
-0.549863096210348));
#28158=CARTESIAN_POINT('Ctrl Pts',(-0.214171831893926,0.141321641909776,
-0.55214747050768));
#28159=CARTESIAN_POINT('Ctrl Pts',(-0.160766372533128,0.187188730027863,
-0.554431844805011));
#28160=CARTESIAN_POINT('Ctrl Pts',(-0.0990433390599819,0.240199336979155,
-0.557071996446939));
#28161=CARTESIAN_POINT('Ctrl Pts',(-0.00852155480020805,0.259678046051574,
-0.559712148088867));
#28162=CARTESIAN_POINT('Ctrl Pts',(0.0695427471374144,0.236747235480135,
-0.562352299730796));
#28163=CARTESIAN_POINT('Ctrl Pts',(0.147607049075037,0.213816424908696,
-0.564992451372724));
#28164=CARTESIAN_POINT('Ctrl Pts',(0.213213868690508,0.148476094693399,
-0.567632603014654));
#28165=CARTESIAN_POINT('Ctrl Pts',(0.236462223963698,0.0705057715725927,
-0.570272754656582));
#28166=CARTESIAN_POINT('Ctrl Pts',(0.259710579236889,-0.00746455154821403,
-0.572912906298511));
#28167=CARTESIAN_POINT('Ctrl Pts',(0.240600470167799,-0.0980648675745309,
-0.575553057940439));
#28168=CARTESIAN_POINT('Ctrl Pts',(0.18784152528326,-0.160003151738218,
-0.578193209582367));
#28169=CARTESIAN_POINT('Ctrl Pts',(0.13508258039872,-0.221941435901907,
-0.580833361224296));
#28170=CARTESIAN_POINT('Ctrl Pts',(0.0486747996987275,-0.255217688202964,
-0.583473512866225));
#28171=CARTESIAN_POINT('Ctrl Pts',(-0.0320005830935595,-0.244665914807472,
-0.586113664508154));
#28172=CARTESIAN_POINT('Ctrl Pts',(-0.112675965885844,-0.23411414141198,
-0.588753816150082));
#28173=CARTESIAN_POINT('Ctrl Pts',(-0.187618950770424,-0.17973434231994,
-0.591393967792011));
#28174=CARTESIAN_POINT('Ctrl Pts',(-0.222673502495132,-0.106310669612487,
-0.59403411943394));
#28175=CARTESIAN_POINT('Ctrl Pts',(-0.238361294687702,-0.0734517322483565,
-0.595215653593632));
#28176=CARTESIAN_POINT('Ctrl Pts',(-0.246060282304069,-0.0367787121380407,
-0.596397187753325));
#28177=CARTESIAN_POINT('Ctrl Pts',(-0.245967927871332,-6.88792904169344E-5,
-0.597578721913017));
#28178=CARTESIAN_POINT('Ctrl Pts',(-0.245979910166711,-8.79836153418138E-5,
-0.604721278086982));
#28179=CARTESIAN_POINT('Ctrl Pts',(-0.246094172159986,-0.0355400995276661,
-0.603580085481056));
#28180=CARTESIAN_POINT('Ctrl Pts',(-0.238932254481067,-0.0709482111534824,
-0.60243889287513));
#28181=CARTESIAN_POINT('Ctrl Pts',(-0.224264499901541,-0.10291199412558,
-0.601297700269203));
#28182=CARTESIAN_POINT('Ctrl Pts',(-0.190330616930831,-0.17686027740204,
-0.598657548627275));
#28183=CARTESIAN_POINT('Ctrl Pts',(-0.116223298799597,-0.232373505977202,
-0.596017396985346));
#28184=CARTESIAN_POINT('Ctrl Pts',(-0.0357177170523464,-0.244150955639253,
-0.593377245343418));
#28185=CARTESIAN_POINT('Ctrl Pts',(0.0447878646949057,-0.255928405301304,
-0.590737093701489));
#28186=CARTESIAN_POINT('Ctrl Pts',(0.131691710058175,-0.223970076050241,
-0.58809694205956));
#28187=CARTESIAN_POINT('Ctrl Pts',(0.185386498747934,-0.162841304750895,
-0.585456790417632));
#28188=CARTESIAN_POINT('Ctrl Pts',(0.239081287437692,-0.10171253345155,
-0.582816638775703));
#28189=CARTESIAN_POINT('Ctrl Pts',(0.259567019453941,-0.011413320103922,
-0.580176487133774));
#28190=CARTESIAN_POINT('Ctrl Pts',(0.237507111979875,0.0669015411628969,
-0.577536335491846));
#28191=CARTESIAN_POINT('Ctrl Pts',(0.215447204505809,0.145216402429716,
-0.574896183849917));
#28192=CARTESIAN_POINT('Ctrl Pts',(0.150841657541429,0.211546911615725,
-0.572256032207989));
#28193=CARTESIAN_POINT('Ctrl Pts',(0.0731351128100314,0.235662257744544,
-0.56961588056606));
#28194=CARTESIAN_POINT('Ctrl Pts',(-0.00457143192136621,0.259777603873362,
-0.566975728924132));
#28195=CARTESIAN_POINT('Ctrl Pts',(-0.0953789744197813,0.24167778694499,
-0.564335577282203));
#28196=CARTESIAN_POINT('Ctrl Pts',(-0.157901044323573,0.189611984464371,
-0.561695425640274));
#28197=CARTESIAN_POINT('Ctrl Pts',(-0.212953202934656,0.143766816177604,
-0.559370709789177));
#28198=CARTESIAN_POINT('Ctrl Pts',(-0.24607501730235,0.0715870779721306,
-0.55704599393808));
#28199=CARTESIAN_POINT('Ctrl Pts',(-0.246614023415026,-0.000159075665185677,
-0.554721278086982));
#28200=CARTESIAN_POINT('Origin',(0.,0.,-0.58));
#28201=CARTESIAN_POINT('',(-0.246483938463648,0.00020522848325015,-0.497578721913017));
#28202=CARTESIAN_POINT('',(-0.246447022145754,0.000212618034880898,-0.504721278086982));
#28203=CARTESIAN_POINT('',(-0.24635,-3.0169173896995E-17,-0.58));
#28204=CARTESIAN_POINT('Ctrl Pts',(-0.246483938463648,0.00020522848325015,
-0.497578721913017));
#28205=CARTESIAN_POINT('Ctrl Pts',(-0.246613670338324,0.0147298283212238,
-0.498048701383514));
#28206=CARTESIAN_POINT('Ctrl Pts',(-0.245439652456884,0.0292334866156357,
-0.498518680854012));
#28207=CARTESIAN_POINT('Ctrl Pts',(-0.242886894023589,0.0434902736077678,
-0.498988660324509));
#28208=CARTESIAN_POINT('Ctrl Pts',(-0.228546545578205,0.123579047583505,
-0.501628811966438));
#28209=CARTESIAN_POINT('Ctrl Pts',(-0.170696854848679,0.195877227472071,
-0.504268963608366));
#28210=CARTESIAN_POINT('Ctrl Pts',(-0.0957034126762081,0.227434175068375,
-0.506909115250295));
#28211=CARTESIAN_POINT('Ctrl Pts',(-0.0207099705037368,0.258991122664679,
-0.509549266892224));
#28212=CARTESIAN_POINT('Ctrl Pts',(0.0714272231116802,0.249806837968721,
-0.512189418534152));
#28213=CARTESIAN_POINT('Ctrl Pts',(0.138715695652291,0.204067153081053,
-0.514829570176081));
#28214=CARTESIAN_POINT('Ctrl Pts',(0.206004168192901,0.158327468193386,
-0.51746972181801));
#28215=CARTESIAN_POINT('Ctrl Pts',(0.248443919658705,0.0760323831140095,
-0.520109873459938));
#28216=CARTESIAN_POINT('Ctrl Pts',(0.246692597334613,-0.00531127171283383,
-0.522750025101867));
#28217=CARTESIAN_POINT('Ctrl Pts',(0.244941275010521,-0.0866549265396772,
-0.525390176743795));
#28218=CARTESIAN_POINT('Ctrl Pts',(0.198998878896533,-0.167047151113988,
-0.528030328385724));
#28219=CARTESIAN_POINT('Ctrl Pts',(0.129804127988899,-0.209848363214838,
-0.530670480027653));
#28220=CARTESIAN_POINT('Ctrl Pts',(0.0606093770812643,-0.252649575315688,
-0.533310631669581));
#28221=CARTESIAN_POINT('Ctrl Pts',(-0.031837728620016,-0.257859774943077,
-0.53595078331151));
#28222=CARTESIAN_POINT('Ctrl Pts',(-0.105403470980325,-0.223104360092322,
-0.538590934953439));
#28223=CARTESIAN_POINT('Ctrl Pts',(-0.178969213340635,-0.188348945241567,
-0.541231086595367));
#28224=CARTESIAN_POINT('Ctrl Pts',(-0.233653592359973,-0.113627915912667,
-0.543871238237295));
#28225=CARTESIAN_POINT('Ctrl Pts',(-0.244533640526383,-0.032996148833134,
-0.546511389879224));
#28226=CARTESIAN_POINT('Ctrl Pts',(-0.245999796706303,-0.0221305017520405,
-0.546867167223822));
#28227=CARTESIAN_POINT('Ctrl Pts',(-0.246670497393433,-0.011157519877363,
-0.547222944568419));
#28228=CARTESIAN_POINT('Ctrl Pts',(-0.246582462449767,-0.000173722512632146,
-0.547578721913017));
#28229=CARTESIAN_POINT('Ctrl Pts',(-0.246614023415026,-0.000159075665185677,
-0.554721278086982));
#28230=CARTESIAN_POINT('Ctrl Pts',(-0.246687160017649,-0.00989415993408876,
-0.554405842296151));
#28231=CARTESIAN_POINT('Ctrl Pts',(-0.246160407898964,-0.0196212613891677,
-0.55409040650532));
#28232=CARTESIAN_POINT('Ctrl Pts',(-0.245007155314066,-0.0292735084317024,
-0.553774970714488));
#28233=CARTESIAN_POINT('Ctrl Pts',(-0.235354599091597,-0.110061410814284,
-0.55113481907256));
#28234=CARTESIAN_POINT('Ctrl Pts',(-0.181812889337495,-0.18560542754658,
-0.548494667430631));
#28235=CARTESIAN_POINT('Ctrl Pts',(-0.108784210307416,-0.221475596937413,
-0.545854515788702));
#28236=CARTESIAN_POINT('Ctrl Pts',(-0.0357555312773367,-0.257345766328247,
-0.543214364146774));
#28237=CARTESIAN_POINT('Ctrl Pts',(0.0567601170287202,-0.253542088377617,
-0.540574212504845));
#28238=CARTESIAN_POINT('Ctrl Pts',(0.12659777747987,-0.211798128386795,
-0.537934060862917));
#28239=CARTESIAN_POINT('Ctrl Pts',(0.19643543793102,-0.170054168395972,
-0.535293909220988));
#28240=CARTESIAN_POINT('Ctrl Pts',(0.243595110527264,-0.090369926364956,
-0.532653757579059));
#28241=CARTESIAN_POINT('Ctrl Pts',(0.246583290010452,-0.0090623141974485,
-0.530013605937131));
#28242=CARTESIAN_POINT('Ctrl Pts',(0.24957146949364,0.0722452979700579,
-0.527373454295202));
#28243=CARTESIAN_POINT('Ctrl Pts',(0.208388155863774,0.155176280274057,
-0.524733302653273));
#28244=CARTESIAN_POINT('Ctrl Pts',(0.141803067384801,0.201933985577598,
-0.522093151011345));
#28245=CARTESIAN_POINT('Ctrl Pts',(0.0752179789058258,0.24869169088114,
-0.519452999369416));
#28246=CARTESIAN_POINT('Ctrl Pts',(-0.0167688844222544,0.259276119184221,
-0.516812847727488));
#28247=CARTESIAN_POINT('Ctrl Pts',(-0.0922335646544927,0.228863308553637,
-0.514172696085559));
#28248=CARTESIAN_POINT('Ctrl Pts',(-0.167698244886729,0.198450497923054,
-0.51153254444363));
#28249=CARTESIAN_POINT('Ctrl Pts',(-0.226640742023121,0.127040448358805,
-0.508892392801702));
#28250=CARTESIAN_POINT('Ctrl Pts',(-0.24219740747612,0.0471790235468913,
-0.506252241159773));
#28251=CARTESIAN_POINT('Ctrl Pts',(-0.24520439136372,0.0317424238221111,
-0.50574192013551));
#28252=CARTESIAN_POINT('Ctrl Pts',(-0.246590397311392,0.0159900644977801,
-0.505231599111246));
#28253=CARTESIAN_POINT('Ctrl Pts',(-0.246447022145754,0.000212618034880898,
-0.504721278086982));
#28254=CARTESIAN_POINT('Origin',(0.,0.,-0.58));
#28255=CARTESIAN_POINT('',(-0.245950337987333,1.22903161040577E-5,-0.447578721913017));
#28256=CARTESIAN_POINT('',(-0.245950012479873,-8.08252214897014E-6,-0.454721278086982));
#28257=CARTESIAN_POINT('',(-0.24635,-3.0169173896995E-17,-0.58));
#28258=CARTESIAN_POINT('Ctrl Pts',(-0.245950337987333,1.22903161040577E-5,
-0.447578721913017));
#28259=CARTESIAN_POINT('Ctrl Pts',(-0.245968336645111,0.0402775323416728,
-0.448874458198609));
#28260=CARTESIAN_POINT('Ctrl Pts',(-0.236630669927586,0.0805349102977895,
-0.450170194484202));
#28261=CARTESIAN_POINT('Ctrl Pts',(-0.217891563823453,0.115795999937283,
-0.451465930769794));
#28262=CARTESIAN_POINT('Ctrl Pts',(-0.179709348584739,0.187642890962127,
-0.454106082411723));
#28263=CARTESIAN_POINT('Ctrl Pts',(-0.102495308803444,0.238746761591991,
-0.456746234053651));
#28264=CARTESIAN_POINT('Ctrl Pts',(-0.0214405363315153,0.245816497796063,
-0.45938638569558));
#28265=CARTESIAN_POINT('Ctrl Pts',(0.0596142361404157,0.252886234000135,
-0.462026537337508));
#28266=CARTESIAN_POINT('Ctrl Pts',(0.144509741302979,0.215921835778419,
-0.464666688979437));
#28267=CARTESIAN_POINT('Ctrl Pts',(0.194553980544851,0.151770207356578,
-0.467306840621366));
#28268=CARTESIAN_POINT('Ctrl Pts',(0.244598219786722,0.0876185789347377,
-0.469946992263295));
#28269=CARTESIAN_POINT('Ctrl Pts',(0.259791193107898,-0.00372027968722727,
-0.472587143905223));
#28270=CARTESIAN_POINT('Ctrl Pts',(0.233208546839486,-0.0806177453661419,
-0.475227295547151));
#28271=CARTESIAN_POINT('Ctrl Pts',(0.206625900571073,-0.15751521104506,
-0.47786744718908));
#28272=CARTESIAN_POINT('Ctrl Pts',(0.138267634713071,-0.219971283780928,
-0.480507598831009));
#28273=CARTESIAN_POINT('Ctrl Pts',(0.0592887311763125,-0.239520966811692,
-0.483147750472938));
#28274=CARTESIAN_POINT('Ctrl Pts',(-0.0196901723604435,-0.259070649842456,
-0.485787902114866));
#28275=CARTESIAN_POINT('Ctrl Pts',(-0.109289713575953,-0.235713943168118,
-0.488428053756795));
#28276=CARTESIAN_POINT('Ctrl Pts',(-0.168673981103086,-0.180095905799495,
-0.491068205398723));
#28277=CARTESIAN_POINT('Ctrl Pts',(-0.217487118485629,-0.134378563276385,
-0.493238377570155));
#28278=CARTESIAN_POINT('Ctrl Pts',(-0.245884889948035,-0.0668634082301429,
-0.495408549741586));
#28279=CARTESIAN_POINT('Ctrl Pts',(-0.246483938463648,0.00020522848325015,
-0.497578721913017));
#28280=CARTESIAN_POINT('Ctrl Pts',(-0.246447022145754,0.000212618034880898,
-0.504721278086982));
#28281=CARTESIAN_POINT('Ctrl Pts',(-0.245848644256014,-0.065634734802945,
-0.502591447469317));
#28282=CARTESIAN_POINT('Ctrl Pts',(-0.218611204094641,-0.131919060374852,
-0.500461616851652));
#28283=CARTESIAN_POINT('Ctrl Pts',(-0.171393337184106,-0.17750991076525,
-0.498331786233988));
#28284=CARTESIAN_POINT('Ctrl Pts',(-0.112861767669489,-0.2340246202059,
-0.495691634592059));
#28285=CARTESIAN_POINT('Ctrl Pts',(-0.0236277948706488,-0.25874123902762,
-0.49305148295013));
#28286=CARTESIAN_POINT('Ctrl Pts',(0.0556392814066714,-0.240394914288013,
-0.490411331308201));
#28287=CARTESIAN_POINT('Ctrl Pts',(0.13490635768399,-0.222048589548406,
-0.487771179666273));
#28288=CARTESIAN_POINT('Ctrl Pts',(0.20420653743979,-0.160639321247473,
-0.485131028024344));
#28289=CARTESIAN_POINT('Ctrl Pts',(0.231955551828012,-0.0841550142722008,
-0.482490876382416));
#28290=CARTESIAN_POINT('Ctrl Pts',(0.259704566216234,-0.00767070729692744,
-0.479850724740487));
#28291=CARTESIAN_POINT('Ctrl Pts',(0.245902415236877,0.0838886383526858,
-0.477210573098558));
#28292=CARTESIAN_POINT('Ctrl Pts',(0.196839570988601,0.148793910305548,
-0.47457042145663));
#28293=CARTESIAN_POINT('Ctrl Pts',(0.147776726740325,0.213699182258409,
-0.471930269814701));
#28294=CARTESIAN_POINT('Ctrl Pts',(0.0634531892231296,0.251950380514519,
-0.469290118172773));
#28295=CARTESIAN_POINT('Ctrl Pts',(-0.0176997230818681,0.24611412851321,
-0.466649966530844));
#28296=CARTESIAN_POINT('Ctrl Pts',(-0.0988526353868669,0.240277876511901,
-0.464009814888915));
#28297=CARTESIAN_POINT('Ctrl Pts',(-0.176834922479668,0.190354174253172,
-0.461369663246987));
#28298=CARTESIAN_POINT('Ctrl Pts',(-0.216105355903885,0.119096261908789,
-0.458729511605058));
#28299=CARTESIAN_POINT('Ctrl Pts',(-0.235978591594914,0.0830354099295665,
-0.457393433765699));
#28300=CARTESIAN_POINT('Ctrl Pts',(-0.245937808335925,0.0415109145690796,
-0.456057355926341));
#28301=CARTESIAN_POINT('Ctrl Pts',(-0.245950012479873,-8.08252214897014E-6,
-0.454721278086982));
#28302=CARTESIAN_POINT('Origin',(0.,0.,-0.58));
#28303=CARTESIAN_POINT('',(-0.246439321146211,-0.000213893874535243,-0.397578721913017));
#28304=CARTESIAN_POINT('',(-0.24647636517194,-0.000206920082869883,-0.404721278086982));
#28305=CARTESIAN_POINT('',(-0.24635,-3.0169173896995E-17,-0.58));
#28306=CARTESIAN_POINT('Ctrl Pts',(-0.246439321146211,-0.000213893874535243,
-0.397578721913017));
#28307=CARTESIAN_POINT('Ctrl Pts',(-0.245841811704369,0.065380979190444,
-0.399700215013704));
#28308=CARTESIAN_POINT('Ctrl Pts',(-0.21884049345472,0.131410332468187,
-0.401821708114392));
#28309=CARTESIAN_POINT('Ctrl Pts',(-0.171950437287423,0.17697032040308,
-0.403943201215079));
#28310=CARTESIAN_POINT('Ctrl Pts',(-0.113596790631628,0.233668726310498,
-0.406583352857008));
#28311=CARTESIAN_POINT('Ctrl Pts',(-0.0244409450267208,0.258665700670919,
-0.409223504498936));
#28312=CARTESIAN_POINT('Ctrl Pts',(0.0548834069927918,0.240568615625082,
-0.411863656140865));
#28313=CARTESIAN_POINT('Ctrl Pts',(0.134207759012302,0.222471530579245,
-0.414503807782794));
#28314=CARTESIAN_POINT('Ctrl Pts',(0.20370061744642,0.161280386127154,-0.417143959424722));
#28315=CARTESIAN_POINT('Ctrl Pts',(0.231689898162049,0.0848836749708929,
-0.419784111066651));
#28316=CARTESIAN_POINT('Ctrl Pts',(0.259679178877679,0.00848696381463214,
-0.422424262708579));
#28317=CARTESIAN_POINT('Ctrl Pts',(0.246164881874822,-0.0831153140457956,
-0.425064414350508));
#28318=CARTESIAN_POINT('Ctrl Pts',(0.197306286845217,-0.148174479443182,
-0.427704565992436));
#28319=CARTESIAN_POINT('Ctrl Pts',(0.148447691815611,-0.213233644840569,
-0.430344717634365));
#28320=CARTESIAN_POINT('Ctrl Pts',(0.064244798759254,-0.251749697774912,
-0.432984869276294));
#28321=CARTESIAN_POINT('Ctrl Pts',(-0.0169260587951456,-0.246168551445078,
-0.435625020918222));
#28322=CARTESIAN_POINT('Ctrl Pts',(-0.0980969163495463,-0.240587405115244,
-0.438265172560151));
#28323=CARTESIAN_POINT('Ctrl Pts',(-0.176235738401991,-0.190909059521233,
-0.440905324202079));
#28324=CARTESIAN_POINT('Ctrl Pts',(-0.215729954080146,-0.119774931014312,
-0.443545475844008));
#28325=CARTESIAN_POINT('Ctrl Pts',(-0.235841158755259,-0.0835520818394694,
-0.444889891200344));
#28326=CARTESIAN_POINT('Ctrl Pts',(-0.245931663144173,-0.0417656627347477,
-0.446234306556681));
#28327=CARTESIAN_POINT('Ctrl Pts',(-0.245950337987333,1.22903161040577E-5,
-0.447578721913017));
#28328=CARTESIAN_POINT('Ctrl Pts',(-0.245950012479873,-8.08252214897014E-6,
-0.454721278086982));
#28329=CARTESIAN_POINT('Ctrl Pts',(-0.245961924289152,-0.0405325451100766,
-0.453417204284412));
#28330=CARTESIAN_POINT('Ctrl Pts',(-0.236497652040484,-0.0810517696819681,
-0.452113130481842));
#28331=CARTESIAN_POINT('Ctrl Pts',(-0.217526516708852,-0.116480294382806,
-0.450809056679272));
#28332=CARTESIAN_POINT('Ctrl Pts',(-0.179118664333969,-0.188206815899989,
-0.448168905037344));
#28333=CARTESIAN_POINT('Ctrl Pts',(-0.101744379828568,-0.239067736504317,
-0.445528753395415));
#28334=CARTESIAN_POINT('Ctrl Pts',(-0.0206677882238031,-0.245882669134951,
-0.442888601753486));
#28335=CARTESIAN_POINT('Ctrl Pts',(0.0604088033809579,-0.252697601765584,
-0.440248450111558));
#28336=CARTESIAN_POINT('Ctrl Pts',(0.14518770208508,-0.215466546422527,
-0.437608298469629));
#28337=CARTESIAN_POINT('Ctrl Pts',(0.195030053868572,-0.151157939053871,
-0.4349681468277));
#28338=CARTESIAN_POINT('Ctrl Pts',(0.244872405652064,-0.0868493316852137,
-0.432327995185772));
#28339=CARTESIAN_POINT('Ctrl Pts',(0.259778210514923,0.00453682770904573,
-0.429687843543843));
#28340=CARTESIAN_POINT('Ctrl Pts',(0.232953994763222,0.0813503581728361,
-0.427047691901915));
#28341=CARTESIAN_POINT('Ctrl Pts',(0.20612977901152,0.158163888636627,-0.424407540259986));
#28342=CARTESIAN_POINT('Ctrl Pts',(0.137575542645258,0.220404790169951,
-0.421767388618057));
#28343=CARTESIAN_POINT('Ctrl Pts',(0.0585355831476179,0.239706132496772,
-0.419127236976129));
#28344=CARTESIAN_POINT('Ctrl Pts',(-0.0205043763500208,0.259007474823592,
-0.4164870853342));
#28345=CARTESIAN_POINT('Ctrl Pts',(-0.110030058979036,0.235369257943911,
-0.413846933692272));
#28346=CARTESIAN_POINT('Ctrl Pts',(-0.169239215181842,0.179564842036591,
-0.411206782050343));
#28347=CARTESIAN_POINT('Ctrl Pts',(-0.217721432531556,0.133870527261602,
-0.409044947395889));
#28348=CARTESIAN_POINT('Ctrl Pts',(-0.245876960799228,0.0666093509869193,
-0.406883112741436));
#28349=CARTESIAN_POINT('Ctrl Pts',(-0.24647636517194,-0.000206920082869883,
-0.404721278086982));
#28350=CARTESIAN_POINT('Origin',(0.,0.,-0.58));
#28351=CARTESIAN_POINT('',(-0.246620278596279,0.000155836006318556,-0.347578721913017));
#28352=CARTESIAN_POINT('',(-0.246589150649816,0.000170838254374723,-0.354721278086982));
#28353=CARTESIAN_POINT('',(-0.24635,-3.0169173896995E-17,-0.58));
#28354=CARTESIAN_POINT('Ctrl Pts',(-0.246620278596279,0.000155836006318556,
-0.347578721913017));
#28355=CARTESIAN_POINT('Ctrl Pts',(-0.246690378530408,0.00963297541655684,
-0.34788582018687));
#28356=CARTESIAN_POINT('Ctrl Pts',(-0.2461911898936,0.0191026624362393,
-0.348192918460724));
#28357=CARTESIAN_POINT('Ctrl Pts',(-0.245097962003322,0.028503266632493,
-0.348500016734578));
#28358=CARTESIAN_POINT('Ctrl Pts',(-0.235699382931871,0.10932111133222,
-0.351140168376506));
#28359=CARTESIAN_POINT('Ctrl Pts',(-0.182395383747831,0.185033047007441,
-0.353780320018435));
#28360=CARTESIAN_POINT('Ctrl Pts',(-0.109479809672547,0.221132581183705,
-0.356420471660364));
#28361=CARTESIAN_POINT('Ctrl Pts',(-0.0365642355972628,0.257232115359969,
-0.359060623302293));
#28362=CARTESIAN_POINT('Ctrl Pts',(0.0559629133692657,0.253719248037275,
-0.361700774944221));
#28363=CARTESIAN_POINT('Ctrl Pts',(0.125931438551998,0.21219500458571,-0.364340926586149));
#28364=CARTESIAN_POINT('Ctrl Pts',(0.195899963734732,0.170670761134143,
-0.366981078228078));
#28365=CARTESIAN_POINT('Ctrl Pts',(0.243309865133668,0.0911351415537013,
-0.369621229870007));
#28366=CARTESIAN_POINT('Ctrl Pts',(0.246553593143224,0.00983732153943592,
-0.372261381511935));
#28367=CARTESIAN_POINT('Ctrl Pts',(0.249797321152781,-0.0714604984748272,
-0.374901533153864));
#28368=CARTESIAN_POINT('Ctrl Pts',(0.208874875772961,-0.154520518922914,
-0.377541684795793));
#28369=CARTESIAN_POINT('Ctrl Pts',(0.142437081882846,-0.201487282208094,
-0.380181836437721));
#28370=CARTESIAN_POINT('Ctrl Pts',(0.0759992879927318,-0.248454045493275,
-0.38282198807965));
#28371=CARTESIAN_POINT('Ctrl Pts',(-0.0159538544076767,-0.259327551615548,
-0.385462139721579));
#28372=CARTESIAN_POINT('Ctrl Pts',(-0.091513756032631,-0.229152088455909,
-0.388102291363507));
#28373=CARTESIAN_POINT('Ctrl Pts',(-0.167073657657585,-0.19897662529627,
-0.390742443005436));
#28374=CARTESIAN_POINT('Ctrl Pts',(-0.226240318507085,-0.127752192854718,
-0.393382594647364));
#28375=CARTESIAN_POINT('Ctrl Pts',(-0.242047925078493,-0.047940057906735,
-0.396022746289293));
#28376=CARTESIAN_POINT('Ctrl Pts',(-0.245153333887077,-0.0322609412877993,
-0.396541404830534));
#28377=CARTESIAN_POINT('Ctrl Pts',(-0.246585399102055,-0.0162504019196318,
-0.397060063371776));
#28378=CARTESIAN_POINT('Ctrl Pts',(-0.246439321146211,-0.000213893874535243,
-0.397578721913017));
#28379=CARTESIAN_POINT('Ctrl Pts',(-0.24647636517194,-0.000206920082869883,
-0.404721278086982));
#28380=CARTESIAN_POINT('Ctrl Pts',(-0.246608986458792,-0.0149903622053166,
-0.404242961099507));
#28381=CARTESIAN_POINT('Ctrl Pts',(-0.245392629983733,-0.0297520245146864,
-0.403764644112032));
#28382=CARTESIAN_POINT('Ctrl Pts',(-0.242748991676294,-0.044253491287515,
-0.403286327124557));
#28383=CARTESIAN_POINT('Ctrl Pts',(-0.228156982191341,-0.124296793769336,
-0.400646175482628));
#28384=CARTESIAN_POINT('Ctrl Pts',(-0.170080333444842,-0.196412783798022,
-0.398006023840699));
#28385=CARTESIAN_POINT('Ctrl Pts',(-0.0949880747257705,-0.227733858068762,
-0.395365872198771));
#28386=CARTESIAN_POINT('Ctrl Pts',(-0.019895816006696,-0.259054932339504,
-0.392725720556842));
#28387=CARTESIAN_POINT('Ctrl Pts',(0.072212052684949,-0.249581090852299,
-0.390085568914914));
#28388=CARTESIAN_POINT('Ctrl Pts',(0.139356423966682,-0.203630134189933,
-0.387445417272985));
#28389=CARTESIAN_POINT('Ctrl Pts',(0.206500795248412,-0.157679177527568,
-0.384805265631057));
#28390=CARTESIAN_POINT('Ctrl Pts',(0.248681669120229,-0.0752511056900446,
-0.382165113989128));
#28391=CARTESIAN_POINT('Ctrl Pts',(0.246674678989956,0.00608664079719441,
-0.379524962347199));
#28392=CARTESIAN_POINT('Ctrl Pts',(0.244667688859683,0.0874243872844334,
-0.376884810705271));
#28393=CARTESIAN_POINT('Ctrl Pts',(0.19847283472732,0.167671808421389,-0.374244659063342));
#28394=CARTESIAN_POINT('Ctrl Pts',(0.1291438959245,0.210255317641276,-0.371604507421414));
#28395=CARTESIAN_POINT('Ctrl Pts',(0.0598149571216795,0.252838826861163,
-0.368964355779485));
#28396=CARTESIAN_POINT('Ctrl Pts',(-0.0326480663515998,0.257758424163981,
-0.366324204137556));
#28397=CARTESIAN_POINT('Ctrl Pts',(-0.106104201672608,0.222771952539835,
-0.363684052495628));
#28398=CARTESIAN_POINT('Ctrl Pts',(-0.179560336993617,0.187785480915688,
-0.361043900853699));
#28399=CARTESIAN_POINT('Ctrl Pts',(-0.234009584162354,0.112892940364575,
-0.358403749211771));
#28400=CARTESIAN_POINT('Ctrl Pts',(-0.244636139423289,0.0322273756154709,
-0.355763597569842));
#28401=CARTESIAN_POINT('Ctrl Pts',(-0.246034577478672,0.0216119134328442,
-0.355416157742222));
#28402=CARTESIAN_POINT('Ctrl Pts',(-0.246674087650934,0.0108964731602588,
-0.355068717914602));
#28403=CARTESIAN_POINT('Ctrl Pts',(-0.246589150649816,0.000170838254374723,
-0.354721278086982));
#28404=CARTESIAN_POINT('Origin',(0.,0.,-0.58));
#28405=CARTESIAN_POINT('',(-0.245982758627801,9.18475011218029E-5,-0.297578721913017));
#28406=CARTESIAN_POINT('',(-0.245970157583507,7.28788751880308E-5,-0.304721278086982));
#28407=CARTESIAN_POINT('',(-0.24635,-3.0169173896995E-17,-0.58));
#28408=CARTESIAN_POINT('Ctrl Pts',(-0.245982758627801,9.18475011218029E-5,
-0.297578721913017));
#28409=CARTESIAN_POINT('Ctrl Pts',(-0.246101246457855,0.0352839351195487,
-0.298711577001966));
#28410=CARTESIAN_POINT('Ctrl Pts',(-0.239047653887906,0.0704307209063493,
-0.299844432090914));
#28411=CARTESIAN_POINT('Ctrl Pts',(-0.224586866480519,0.102206587808051,
-0.300977287179863));
#28412=CARTESIAN_POINT('Ctrl Pts',(-0.190885582009419,0.176261167244235,
-0.303617438821791));
#28413=CARTESIAN_POINT('Ctrl Pts',(-0.116953115508088,0.232007054354664,
-0.30625759046372));
#28414=CARTESIAN_POINT('Ctrl Pts',(-0.0364849480944337,0.24403748840998,
-0.308897742105649));
#28415=CARTESIAN_POINT('Ctrl Pts',(0.0439832193192205,0.256067922465295,
-0.311537893747577));
#28416=CARTESIAN_POINT('Ctrl Pts',(0.130987087645194,0.224382903465497,
-0.314178045389506));
#28417=CARTESIAN_POINT('Ctrl Pts',(0.184873750101168,0.163423204320673,
-0.316818197031434));
#28418=CARTESIAN_POINT('Ctrl Pts',(0.238760412557142,0.102463505175849,
-0.319458348673363));
#28419=CARTESIAN_POINT('Ctrl Pts',(0.259529869143112,0.0122291258859946,
-0.322098500315292));
#28420=CARTESIAN_POINT('Ctrl Pts',(0.237716226654917,-0.0661546882076611,
-0.32473865195722));
#28421=CARTESIAN_POINT('Ctrl Pts',(0.215902584166721,-0.144538502301317,
-0.327378803599149));
#28422=CARTESIAN_POINT('Ctrl Pts',(0.151505842604362,-0.211071751198777,
-0.330018955241077));
#28423=CARTESIAN_POINT('Ctrl Pts',(0.0738754784841004,-0.235431223217419,
-0.332659106883006));
#28424=CARTESIAN_POINT('Ctrl Pts',(-0.00375488563616382,-0.259790695236061,
-0.335299258524935));
#28425=CARTESIAN_POINT('Ctrl Pts',(-0.0946188723143317,-0.241976390375881,
-0.337939410166864));
#28426=CARTESIAN_POINT('Ctrl Pts',(-0.157304286173984,-0.190107361083673,
-0.340579561808792));
#28427=CARTESIAN_POINT('Ctrl Pts',(-0.212698231586755,-0.144271655449523,
-0.342912615176867));
#28428=CARTESIAN_POINT('Ctrl Pts',(-0.246087723055121,-0.0718428494415446,
-0.345245668544942));
#28429=CARTESIAN_POINT('Ctrl Pts',(-0.246620278596279,0.000155836006318556,
-0.347578721913017));
#28430=CARTESIAN_POINT('Ctrl Pts',(-0.246589150649816,0.000170838254374723,
-0.354721278086982));
#28431=CARTESIAN_POINT('Ctrl Pts',(-0.246028662040124,-0.0706062802847878,
-0.352428566272674));
#28432=CARTESIAN_POINT('Ctrl Pts',(-0.21392201658485,-0.141827325604046,
-0.350135854458365));
#28433=CARTESIAN_POINT('Ctrl Pts',(-0.16017720978418,-0.187693116327548,
-0.347843142644056));
#28434=CARTESIAN_POINT('Ctrl Pts',(-0.0982878615310032,-0.240509454574367,
-0.345202991002127));
#28435=CARTESIAN_POINT('Ctrl Pts',(-0.00770530167151524,-0.259703542120912,
-0.342562839360199));
#28436=CARTESIAN_POINT('Ctrl Pts',(0.0702865375815846,-0.236527476386538,
-0.33992268771827));
#28437=CARTESIAN_POINT('Ctrl Pts',(0.148278376834687,-0.213351410652164,
-0.337282536076342));
#28438=CARTESIAN_POINT('Ctrl Pts',(0.213679495481401,-0.147805191636868,
-0.334642384434413));
#28439=CARTESIAN_POINT('Ctrl Pts',(0.236682661831279,-0.0697621820147013,
-0.332002232792484));
#28440=CARTESIAN_POINT('Ctrl Pts',(0.259685828181155,0.00828082760746218,
-0.329362081150556));
#28441=CARTESIAN_POINT('Ctrl Pts',(0.240291042234199,0.0988206278364971,
-0.326721929508627));
#28442=CARTESIAN_POINT('Ctrl Pts',(0.18733767692882,0.160592774600555,-0.324081777866698));
#28443=CARTESIAN_POINT('Ctrl Pts',(0.134384311623439,0.222364921364616,
-0.32144162622477));
#28444=CARTESIAN_POINT('Ctrl Pts',(0.0478723669596356,0.255369414663697,
-0.318801474582841));
#28445=CARTESIAN_POINT('Ctrl Pts',(-0.0327694495428521,0.24456411762082,
-0.316161322940913));
#28446=CARTESIAN_POINT('Ctrl Pts',(-0.113411266045338,0.233758820577943,
-0.313521171298984));
#28447=CARTESIAN_POINT('Ctrl Pts',(-0.188182954386505,0.179143733193108,
-0.310881019657055));
#28448=CARTESIAN_POINT('Ctrl Pts',(-0.223006549473582,0.105610242604011,
-0.308240868015127));
#28449=CARTESIAN_POINT('Ctrl Pts',(-0.238481010938067,0.0729343754620719,
-0.307067671372412));
#28450=CARTESIAN_POINT('Ctrl Pts',(-0.246067235702702,0.0365228395984935,
-0.305894474729697));
#28451=CARTESIAN_POINT('Ctrl Pts',(-0.245970157583507,7.28788751880308E-5,
-0.304721278086982));
#28452=CARTESIAN_POINT('Origin',(0.,0.,-0.58));
#28453=CARTESIAN_POINT('',(-0.246288309719265,-0.000221392196024267,-0.247578721913017));
#28454=CARTESIAN_POINT('',(-0.246325271707252,-0.000222610671457577,-0.254721278086982));
#28455=CARTESIAN_POINT('',(-0.24635,-3.0169173896995E-17,-0.58));
#28456=CARTESIAN_POINT('Ctrl Pts',(-0.246288309719265,-0.000221392196024267,
-0.247578721913017));
#28457=CARTESIAN_POINT('Ctrl Pts',(-0.245750103398489,0.0604324982965131,
-0.24953733381706));
#28458=CARTESIAN_POINT('Ctrl Pts',(-0.223113577325142,0.121445534342942,
-0.251495945721104));
#28459=CARTESIAN_POINT('Ctrl Pts',(-0.182486358855138,0.1660848458429,-0.253454557625148));
#28460=CARTESIAN_POINT('Ctrl Pts',(-0.127722054947289,0.226257333974859,
-0.256094709267076));
#28461=CARTESIAN_POINT('Ctrl Pts',(-0.0402682085204694,0.256678351015285,
-0.258734860909005));
#28462=CARTESIAN_POINT('Ctrl Pts',(0.0400171915015985,0.243483205932552,
-0.261375012550933));
#28463=CARTESIAN_POINT('Ctrl Pts',(0.12030259152367,0.230288060849818,-0.264015164192862));
#28464=CARTESIAN_POINT('Ctrl Pts',(0.193419545140986,0.173476753643925,
-0.266655315834791));
#28465=CARTESIAN_POINT('Ctrl Pts',(0.226044249609935,0.0989416211976409,
-0.269295467476719));
#28466=CARTESIAN_POINT('Ctrl Pts',(0.258668954078883,0.0244064887513605,
-0.271935619118648));
#28467=CARTESIAN_POINT('Ctrl Pts',(0.250801409399463,-0.0678524689353101,
-0.274575770760577));
#28468=CARTESIAN_POINT('Ctrl Pts',(0.206027329882984,-0.135787284118156,
-0.277215922402505));
#28469=CARTESIAN_POINT('Ctrl Pts',(0.161253250366504,-0.203722099301003,
-0.279856074044434));
#28470=CARTESIAN_POINT('Ctrl Pts',(0.0795726360129633,-0.247332771980028,
-0.282496225686362));
#28471=CARTESIAN_POINT('Ctrl Pts',(-0.00178773407926969,-0.246743290068368,
-0.285136377328291));
#28472=CARTESIAN_POINT('Ctrl Pts',(-0.0831481041715026,-0.246153808156707,
-0.28777652897022));
#28473=CARTESIAN_POINT('Ctrl Pts',(-0.164188230002428,-0.201364171654361,
-0.290416680612148));
#28474=CARTESIAN_POINT('Ctrl Pts',(-0.207973241697457,-0.132787717522219,
-0.293056832254077));
#28475=CARTESIAN_POINT('Ctrl Pts',(-0.232970668417953,-0.0936365372311268,
-0.294564128807057));
#28476=CARTESIAN_POINT('Ctrl Pts',(-0.245825107133315,-0.0467322457804416,
-0.296071425360037));
#28477=CARTESIAN_POINT('Ctrl Pts',(-0.245982758627801,9.18475011218029E-5,
-0.297578721913017));
#28478=CARTESIAN_POINT('Ctrl Pts',(-0.245970157583507,7.28788751880308E-5,
-0.304721278086982));
#28479=CARTESIAN_POINT('Ctrl Pts',(-0.245848771937587,-0.0455038387503123,
-0.303254323087769));
#28480=CARTESIAN_POINT('Ctrl Pts',(-0.233714706137793,-0.0911406328242931,
-0.301787368088555));
#28481=CARTESIAN_POINT('Ctrl Pts',(-0.209968597656244,-0.129609538419296,
-0.300320413089341));
#28482=CARTESIAN_POINT('Ctrl Pts',(-0.16723154891884,-0.198843935060144,
-0.297680261447412));
#28483=CARTESIAN_POINT('Ctrl Pts',(-0.0868819496110477,-0.244860834548482,
-0.295040109805483));
#28484=CARTESIAN_POINT('Ctrl Pts',(-0.00553995505069527,-0.246687562209828,
-0.292399958163555));
#28485=CARTESIAN_POINT('Ctrl Pts',(0.0758020395096583,-0.248514289871173,
-0.289759806521626));
#28486=CARTESIAN_POINT('Ctrl Pts',(0.158136429322571,-0.206150845705526,
-0.287119654879698));
#28487=CARTESIAN_POINT('Ctrl Pts',(0.203938470407728,-0.138904804592017,
-0.284479503237769));
#28488=CARTESIAN_POINT('Ctrl Pts',(0.249740511492885,-0.0716587634785091,
-0.281839351595841));
#28489=CARTESIAN_POINT('Ctrl Pts',(0.259010203850289,0.0204698745828584,
-0.279199199953912));
#28490=CARTESIAN_POINT('Ctrl Pts',(0.227522789960257,0.0954925363559746,
-0.276559048311983));
#28491=CARTESIAN_POINT('Ctrl Pts',(0.196035376070226,0.17051519812909,-0.273918896670055));
#28492=CARTESIAN_POINT('Ctrl Pts',(0.123790855932758,0.228431883613956,
-0.271278745028126));
#28493=CARTESIAN_POINT('Ctrl Pts',(0.0437154117701946,0.242846468421408,
-0.268638593386197));
#28494=CARTESIAN_POINT('Ctrl Pts',(-0.0363600323923712,0.257261053228861,
-0.265998441744269));
#28495=CARTESIAN_POINT('Ctrl Pts',(-0.124266400580035,0.228173537358901,
-0.26335829010234));
#28496=CARTESIAN_POINT('Ctrl Pts',(-0.17993946242722,0.168840854985951,
-0.260718138460411));
#28497=CARTESIAN_POINT('Ctrl Pts',(-0.22209153343667,0.123917954078675,
-0.258719185002602));
#28498=CARTESIAN_POINT('Ctrl Pts',(-0.245765710234638,0.0616568694570882,
-0.256720231544792));
#28499=CARTESIAN_POINT('Ctrl Pts',(-0.246325271707252,-0.000222610671457577,
-0.254721278086982));
#28500=CARTESIAN_POINT('Origin',(0.,0.,-0.58));
#28501=CARTESIAN_POINT('',(-0.246717581299304,8.00647905813846E-5,-0.197578721913017));
#28502=CARTESIAN_POINT('',(-0.246698535278583,0.000100771421362301,-0.204721278086982));
#28503=CARTESIAN_POINT('',(-0.24635,-3.0169173896995E-17,-0.58));
#28504=CARTESIAN_POINT('Ctrl Pts',(-0.246717581299304,8.00647905813846E-5,
-0.197578721913017));
#28505=CARTESIAN_POINT('Ctrl Pts',(-0.246736504680948,0.00452600816889543,
-0.197722938990227));
#28506=CARTESIAN_POINT('Ctrl Pts',(-0.246626683453427,0.00897099792437958,
-0.197867156067437));
#28507=CARTESIAN_POINT('Ctrl Pts',(-0.246385167424414,0.0134088205603487,
-0.198011373144647));
#28508=CARTESIAN_POINT('Ctrl Pts',(-0.241963784375424,0.0946511043842296,
-0.200651524786575));
#28509=CARTESIAN_POINT('Ctrl Pts',(-0.193406398690778,0.173491410284751,
-0.203291676428504));
#28510=CARTESIAN_POINT('Ctrl Pts',(-0.122843537789156,0.213997458887118,
-0.205931828070432));
#28511=CARTESIAN_POINT('Ctrl Pts',(-0.0522806768875334,0.254503507489485,
-0.208571979712361));
#28512=CARTESIAN_POINT('Ctrl Pts',(0.0402876592310675,0.2566752987937,-0.21121213135429));
#28513=CARTESIAN_POINT('Ctrl Pts',(0.112672500456431,0.219523016619024,
-0.213852282996218));
#28514=CARTESIAN_POINT('Ctrl Pts',(0.185057341681796,0.182370734444347,
-0.216492434638147));
#28515=CARTESIAN_POINT('Ctrl Pts',(0.237258688013924,0.105894378790777,
-0.219132586280076));
#28516=CARTESIAN_POINT('Ctrl Pts',(0.2454852395792,0.0249488343818461,-0.221772737922004));
#28517=CARTESIAN_POINT('Ctrl Pts',(0.253711791144477,-0.0559967100270831,
-0.224412889563933));
#28518=CARTESIAN_POINT('Ctrl Pts',(0.217963547942906,-0.141411443191371,
-0.227053041205861));
#28519=CARTESIAN_POINT('Ctrl Pts',(0.154533139065134,-0.192366722999149,
-0.22969319284779));
#28520=CARTESIAN_POINT('Ctrl Pts',(0.0911027301873629,-0.243322002806927,
-0.232333344489719));
#28521=CARTESIAN_POINT('Ctrl Pts',(-9.84436660830812E-6,-0.259817829258193,
-0.234973496131648));
#28522=CARTESIAN_POINT('Ctrl Pts',(-0.0772790927469542,-0.234336059988257,
-0.237613647773576));
#28523=CARTESIAN_POINT('Ctrl Pts',(-0.1545483411273,-0.208854290718321,
-0.240253799415505));
#28524=CARTESIAN_POINT('Ctrl Pts',(-0.217974263334022,-0.141394925727183,
-0.242893951057433));
#28525=CARTESIAN_POINT('Ctrl Pts',(-0.238649843742943,-0.0627032636198674,
-0.245534102699361));
#28526=CARTESIAN_POINT('Ctrl Pts',(-0.243987124158482,-0.042389470307912,
-0.246215642437246));
#28527=CARTESIAN_POINT('Ctrl Pts',(-0.246475589799629,-0.0213271745833612,
-0.246897182175132));
#28528=CARTESIAN_POINT('Ctrl Pts',(-0.246288309719265,-0.000221392196024267,
-0.247578721913017));
#28529=CARTESIAN_POINT('Ctrl Pts',(-0.246325271707252,-0.000222610671457577,
-0.254721278086982));
#28530=CARTESIAN_POINT('Ctrl Pts',(-0.246504760528635,-0.0200715021689657,
-0.254080079902863));
#28531=CARTESIAN_POINT('Ctrl Pts',(-0.244305953528097,-0.0398811298345366,
-0.253438881718744));
#28532=CARTESIAN_POINT('Ctrl Pts',(-0.239575819577798,-0.0590666667812709,
-0.252797683534626));
#28533=CARTESIAN_POINT('Ctrl Pts',(-0.220099359374485,-0.138063657299604,
-0.250157531892697));
#28534=CARTESIAN_POINT('Ctrl Pts',(-0.157706683461156,-0.206479789460333,
-0.247517380250768));
#28535=CARTESIAN_POINT('Ctrl Pts',(-0.080833894847107,-0.233133708190821,
-0.24487722860884));
#28536=CARTESIAN_POINT('Ctrl Pts',(-0.00396110623305791,-0.259787626921309,
-0.242237076966911));
#28537=CARTESIAN_POINT('Ctrl Pts',(0.0873917950817112,-0.244679332221555,
-0.239596925324982));
#28538=CARTESIAN_POINT('Ctrl Pts',(0.151589785853267,-0.194694584608596,
-0.236956773683054));
#28539=CARTESIAN_POINT('Ctrl Pts',(0.215787776624823,-0.144709836995635,
-0.234316622041125));
#28540=CARTESIAN_POINT('Ctrl Pts',(0.252830856853165,-0.0598486364694672,
-0.231676470399197));
#28541=CARTESIAN_POINT('Ctrl Pts',(0.24583626217839,0.0212126530485721,
-0.229036318757268));
#28542=CARTESIAN_POINT('Ctrl Pts',(0.238841667503615,0.10227394256661,-0.22639616711534));
#28543=CARTESIAN_POINT('Ctrl Pts',(0.187809397925725,0.17953532107652,-0.223756015473411));
#28544=CARTESIAN_POINT('Ctrl Pts',(0.115997934563216,0.217784121615343,
-0.221115863831482));
#28545=CARTESIAN_POINT('Ctrl Pts',(0.044186471200707,0.256032922154165,
-0.218475712189554));
#28546=CARTESIAN_POINT('Ctrl Pts',(-0.0484041859464199,0.255269144721901,
-0.215835560547625));
#28547=CARTESIAN_POINT('Ctrl Pts',(-0.119574893702499,0.215840888727965,
-0.213195408905696));
#28548=CARTESIAN_POINT('Ctrl Pts',(-0.190745601458579,0.176412632734028,
-0.210555257263768));
#28549=CARTESIAN_POINT('Ctrl Pts',(-0.240496359823611,0.098319898178419,
-0.207915105621839));
#28550=CARTESIAN_POINT('Ctrl Pts',(-0.246152749572341,0.0171542510864486,
-0.20527495397991));
#28551=CARTESIAN_POINT('Ctrl Pts',(-0.246548156992019,0.0114804024818092,
-0.205090395348934));
#28552=CARTESIAN_POINT('Ctrl Pts',(-0.246728090793561,0.00579153763806257,
-0.204905836717958));
#28553=CARTESIAN_POINT('Ctrl Pts',(-0.246698535278583,0.000100771421362301,
-0.204721278086982));
#28554=CARTESIAN_POINT('Origin',(0.,0.,-0.58));
#28555=CARTESIAN_POINT('',(-0.246061894210452,0.000159263489505596,-0.147578721913017));
#28556=CARTESIAN_POINT('',(-0.246038304346645,0.000144234873082875,-0.154721278086982));
#28557=CARTESIAN_POINT('',(-0.24635,-3.0169173896995E-17,-0.58));
#28558=CARTESIAN_POINT('Ctrl Pts',(-0.246061894210452,0.000159263489505596,
-0.147578721913017));
#28559=CARTESIAN_POINT('Ctrl Pts',(-0.246241265808746,0.0302671727973585,
-0.148548695805322));
#28560=CARTESIAN_POINT('Ctrl Pts',(-0.241124310761266,0.0603162330277041,
-0.149518669697626));
#28561=CARTESIAN_POINT('Ctrl Pts',(-0.230435621126537,0.0882319217573935,
-0.150488643589931));
#28562=CARTESIAN_POINT('Ctrl Pts',(-0.201342300457734,0.164215050808554,
-0.15312879523186));
#28563=CARTESIAN_POINT('Ctrl Pts',(-0.130970083701752,0.224392828920623,
-0.155768946873788));
#28564=CARTESIAN_POINT('Ctrl Pts',(-0.0513918344865268,0.24133861398937,
-0.158409098515717));
#28565=CARTESIAN_POINT('Ctrl Pts',(0.0281864147286988,0.258284399058117,
-0.161049250157646));
#28566=CARTESIAN_POINT('Ctrl Pts',(0.116970696403168,0.231998191083541,
-0.163689401799574));
#28567=CARTESIAN_POINT('Ctrl Pts',(0.174496663610151,0.174460200189865,
-0.166329553441503));
#28568=CARTESIAN_POINT('Ctrl Pts',(0.232022630817135,0.116922209296188,
-0.168969705083432));
#28569=CARTESIAN_POINT('Ctrl Pts',(0.25829028355663,0.0281324354834098,
-0.17160985672536));
#28570=CARTESIAN_POINT('Ctrl Pts',(0.241327868439501,-0.0514422701154425,
-0.174250008367289));
#28571=CARTESIAN_POINT('Ctrl Pts',(0.224365453322372,-0.131016975714293,
-0.176890160009218));
#28572=CARTESIAN_POINT('Ctrl Pts',(0.164172970348623,-0.201376613099217,
-0.179530311651146));
#28573=CARTESIAN_POINT('Ctrl Pts',(0.0881837624159238,-0.230454054503992,
-0.182170463293075));
#28574=CARTESIAN_POINT('Ctrl Pts',(0.012194554483225,-0.259531495908768,
-0.184810614935003));
#28575=CARTESIAN_POINT('Ctrl Pts',(-0.0795913784084228,-0.247326741333394,
-0.187450766576932));
#28576=CARTESIAN_POINT('Ctrl Pts',(-0.14534165464758,-0.199402233172087,
-0.19009091821886));
#28577=CARTESIAN_POINT('Ctrl Pts',(-0.207500352087109,-0.154095579373379,
-0.192586852783579));
#28578=CARTESIAN_POINT('Ctrl Pts',(-0.246390078320868,-0.0768649403738304,
-0.195082787348298));
#28579=CARTESIAN_POINT('Ctrl Pts',(-0.246717581299304,8.00647905813846E-5,
-0.197578721913017));
#28580=CARTESIAN_POINT('Ctrl Pts',(-0.246698535278583,0.000100771421362301,
-0.204721278086982));
#28581=CARTESIAN_POINT('Ctrl Pts',(-0.246305292677956,-0.0756161196000796,
-0.202265685076029));
#28582=CARTESIAN_POINT('Ctrl Pts',(-0.208826396508379,-0.151669608495989,
-0.199810092065077));
#28583=CARTESIAN_POINT('Ctrl Pts',(-0.148357316731195,-0.197168838869184,
-0.197354499054125));
#28584=CARTESIAN_POINT('Ctrl Pts',(-0.0833434730088882,-0.246087722104518,
-0.194714347412196));
#28585=CARTESIAN_POINT('Ctrl Pts',(0.00824623556815356,-0.259686928946854,
-0.192074195770267));
#28586=CARTESIAN_POINT('Ctrl Pts',(0.0846688584477465,-0.231768481161568,
-0.189434044128339));
#28587=CARTESIAN_POINT('Ctrl Pts',(0.161091481327338,-0.203850033376283,
-0.18679389248641));
#28588=CARTESIAN_POINT('Ctrl Pts',(0.222347018509481,-0.134413930963373,
-0.184153740844482));
#28589=CARTESIAN_POINT('Ctrl Pts',(0.240517629577363,-0.0551063909376154,
-0.181513589202553));
#28590=CARTESIAN_POINT('Ctrl Pts',(0.258688240645247,0.024201149088146,
-0.178873437560624));
#28591=CARTESIAN_POINT('Ctrl Pts',(0.233773925598868,0.113380126726757,
-0.176233285918696));
#28592=CARTESIAN_POINT('Ctrl Pts',(0.177129639592286,0.171786306822376,
-0.173593134276767));
#28593=CARTESIAN_POINT('Ctrl Pts',(0.120485353585707,0.230192486917993,
-0.170952982634838));
#28594=CARTESIAN_POINT('Ctrl Pts',(0.0321110966189257,0.257825869470619,
-0.16831283099291));
#28595=CARTESIAN_POINT('Ctrl Pts',(-0.0477156560646856,0.242092256426266,
-0.165672679350981));
#28596=CARTESIAN_POINT('Ctrl Pts',(-0.127542408748298,0.226358643381913,
-0.163032527709053));
#28597=CARTESIAN_POINT('Ctrl Pts',(-0.19882165714874,0.16725803474058,-0.160392376067124));
#28598=CARTESIAN_POINT('Ctrl Pts',(-0.2290671510981,0.0917261401792469,
-0.157752224425195));
#28599=CARTESIAN_POINT('Ctrl Pts',(-0.240641292986694,0.0628221035571004,
-0.156741908979124));
#28600=CARTESIAN_POINT('Ctrl Pts',(-0.246206500009256,0.0315118887000048,
-0.155731593533053));
#28601=CARTESIAN_POINT('Ctrl Pts',(-0.246038304346645,0.000144234873082875,
-0.154721278086982));
#28602=CARTESIAN_POINT('Origin',(0.,0.,-0.58));
#28603=CARTESIAN_POINT('',(-0.246149652364137,-0.000196946980918933,-0.0975787219130166));
#28604=CARTESIAN_POINT('',(-0.246181916821291,-0.000205804393626753,-0.104721278086982));
#28605=CARTESIAN_POINT('',(-0.24635,-3.0169173896995E-17,-0.58));
#28606=CARTESIAN_POINT('Ctrl Pts',(-0.246149652364137,-0.000196946980918933,
-0.0975787219130166));
#28607=CARTESIAN_POINT('Ctrl Pts',(-0.245729114976462,0.0554922919781312,
-0.0993744526204165));
#28608=CARTESIAN_POINT('Ctrl Pts',(-0.227001298186543,0.111437622002477,
-0.101170183327816));
#28609=CARTESIAN_POINT('Ctrl Pts',(-0.192334463664016,0.154573316616123,
-0.102965914035216));
#28610=CARTESIAN_POINT('Ctrl Pts',(-0.141365963928531,0.217993056831428,
-0.105606065677145));
#28611=CARTESIAN_POINT('Ctrl Pts',(-0.0559436839388203,0.253723489525969,
-0.108246217319073));
#28612=CARTESIAN_POINT('Ctrl Pts',(0.0250001579011069,0.245480031317822,
-0.110886368961002));
#28613=CARTESIAN_POINT('Ctrl Pts',(0.105943999741037,0.237236573109673,
-0.11352652060293));
#28614=CARTESIAN_POINT('Ctrl Pts',(0.182409403431186,0.185019223998827,
-0.116166672244859));
#28615=CARTESIAN_POINT('Ctrl Pts',(0.219546547681062,0.112626614966495,
-0.118806823886788));
#28616=CARTESIAN_POINT('Ctrl Pts',(0.256683691930939,0.0402340059341607,
-0.121446975528716));
#28617=CARTESIAN_POINT('Ctrl Pts',(0.254492576740548,-0.0523338630196622,
-0.124087127170645));
#28618=CARTESIAN_POINT('Ctrl Pts',(0.213971787489004,-0.122888254505354,
-0.126727278812574));
#28619=CARTESIAN_POINT('Ctrl Pts',(0.173450998237462,-0.193442645991044,
-0.129367430454502));
#28620=CARTESIAN_POINT('Ctrl Pts',(0.0946005349247738,-0.241983560008603,
-0.132007582096431));
#28621=CARTESIAN_POINT('Ctrl Pts',(0.0133573261733158,-0.246387965892067,
-0.13464773373836));
#28622=CARTESIAN_POINT('Ctrl Pts',(-0.0678858825781422,-0.250792371775532,
-0.137287885380288));
#28623=CARTESIAN_POINT('Ctrl Pts',(-0.151521836768367,-0.211060269524901,
-0.139928037022217));
#28624=CARTESIAN_POINT('Ctrl Pts',(-0.199432601572667,-0.14529997840446,
-0.142568188664145));
#28625=CARTESIAN_POINT('Ctrl Pts',(-0.229741274784008,-0.103699574361793,
-0.144238366413769));
#28626=CARTESIAN_POINT('Ctrl Pts',(-0.245753038008484,-0.0516829155759291,
-0.145908544163393));
#28627=CARTESIAN_POINT('Ctrl Pts',(-0.246061894210452,0.000159263489505596,
-0.147578721913017));
#28628=CARTESIAN_POINT('Ctrl Pts',(-0.246038304346645,0.000144234873082875,
-0.154721278086982));
#28629=CARTESIAN_POINT('Ctrl Pts',(-0.245766971883129,-0.0504579189245854,
-0.153091441891125));
#28630=CARTESIAN_POINT('Ctrl Pts',(-0.230575036347777,-0.101209551856495,
-0.151461605695267));
#28631=CARTESIAN_POINT('Ctrl Pts',(-0.201619231011091,-0.142250237299355,
-0.149831769499409));
#28632=CARTESIAN_POINT('Ctrl Pts',(-0.154714077476446,-0.208731539735291,
-0.147191617857481));
#28633=CARTESIAN_POINT('Ctrl Pts',(-0.0716920309088846,-0.24973096412583,
-0.144551466215552));
#28634=CARTESIAN_POINT('Ctrl Pts',(0.00960875972723208,-0.246562601087141,
-0.141911314573624));
#28635=CARTESIAN_POINT('Ctrl Pts',(0.0909095503633488,-0.243394238048452,
-0.139271162931695));
#28636=CARTESIAN_POINT('Ctrl Pts',(0.170489085068021,-0.19605808758053,
-0.136631011289766));
#28637=CARTESIAN_POINT('Ctrl Pts',(0.21207817024949,-0.126128087551106,
-0.133990859647838));
#28638=CARTESIAN_POINT('Ctrl Pts',(0.253667255430958,-0.0561980875216845,
-0.131350708005909));
#28639=CARTESIAN_POINT('Ctrl Pts',(0.25726589108923,0.0363257620692371,
-0.128710556363981));
#28640=CARTESIAN_POINT('Ctrl Pts',(0.221233967996605,0.109274768183429,
-0.126070404722052));
#28641=CARTESIAN_POINT('Ctrl Pts',(0.185202044903979,0.182223774297623,
-0.123430253080123));
#28642=CARTESIAN_POINT('Ctrl Pts',(0.109539563060456,0.235597936935084,
-0.120790101438195));
#28643=CARTESIAN_POINT('Ctrl Pts',(0.0287304645584095,0.24507142952619,
-0.118149949796266));
#28644=CARTESIAN_POINT('Ctrl Pts',(-0.052078633943639,0.254544922117296,
-0.115509798154338));
#28645=CARTESIAN_POINT('Ctrl Pts',(-0.138034349104214,0.220117744662039,
-0.112869646512409));
#28646=CARTESIAN_POINT('Ctrl Pts',(-0.189961459263067,0.157480443860448,
-0.11022949487048));
#28647=CARTESIAN_POINT('Ctrl Pts',(-0.226073751091705,0.113919835943204,
-0.108393422609314));
#28648=CARTESIAN_POINT('Ctrl Pts',(-0.245728464227458,0.0567156970941223,
-0.106557350348148));
#28649=CARTESIAN_POINT('Ctrl Pts',(-0.246181916821291,-0.000205804393626753,
-0.104721278086982));
#28650=CARTESIAN_POINT('Origin',(0.,0.,-0.58));
#28651=CARTESIAN_POINT('',(-0.246745528500925,-8.72836701185098E-6,-0.0475787219130168));
#28652=CARTESIAN_POINT('',(-0.246748421001242,1.25335797698571E-5,-0.0547212780869822));
#28653=CARTESIAN_POINT('',(-0.24635,-3.0169173896995E-17,-0.58));
#28654=CARTESIAN_POINT('Ctrl Pts',(-0.246745528500925,-8.72836701185098E-6,
-0.0475787219130168));
#28655=CARTESIAN_POINT('Ctrl Pts',(-0.246691462824838,0.080780672528638,
-0.0502002094355115));
#28656=CARTESIAN_POINT('Ctrl Pts',(-0.203208326166415,0.161612112961239,
-0.0528216969580061));
#28657=CARTESIAN_POINT('Ctrl Pts',(-0.135746111999613,0.206054714378708,
-0.0554431844805008));
#28658=CARTESIAN_POINT('Ctrl Pts',(-0.0678035893012281,0.250813732339722,
-0.0580833361224295));
#28659=CARTESIAN_POINT('Ctrl Pts',(0.0244606725130793,0.258663913880818,
-0.0607234877643582));
#28660=CARTESIAN_POINT('Ctrl Pts',(0.0989898525822783,0.226024087587752,
-0.0633636394062869));
#28661=CARTESIAN_POINT('Ctrl Pts',(0.173519032651475,0.193384261294688,
-0.0660037910482156));
#28662=CARTESIAN_POINT('Ctrl Pts',(0.230313130975565,0.120254427167465,
-0.0686439426901442));
#28663=CARTESIAN_POINT('Ctrl Pts',(0.243491040779466,0.039966032231016,
-0.0712840943320728));
#28664=CARTESIAN_POINT('Ctrl Pts',(0.256668950583366,-0.0403223627054333,
-0.0739242459740013));
#28665=CARTESIAN_POINT('Ctrl Pts',(0.226230671867078,-0.127769318451109,
-0.0765643976159299));
#28666=CARTESIAN_POINT('Ctrl Pts',(0.166046980319095,-0.182520920142066,
-0.0792045492578585));
#28667=CARTESIAN_POINT('Ctrl Pts',(0.105863288771112,-0.237272521833022,
-0.0818447008997871));
#28668=CARTESIAN_POINT('Ctrl Pts',(0.0159341843914353,-0.25932876946926,
-0.0844848525417159));
#28669=CARTESIAN_POINT('Ctrl Pts',(-0.0627532815273662,-0.238636810281684,
-0.0871250041836445));
#28670=CARTESIAN_POINT('Ctrl Pts',(-0.141440747446168,-0.217944851094108,
-0.089765155825573));
#28671=CARTESIAN_POINT('Ctrl Pts',(-0.208886574904093,-0.15450468508272,
-0.0924053074675015));
#28672=CARTESIAN_POINT('Ctrl Pts',(-0.234352128892428,-0.0772300782089907,
-0.0950454591094301));
#28673=CARTESIAN_POINT('Ctrl Pts',(-0.242496981845425,-0.0525147191684789,
-0.0958898800439589));
#28674=CARTESIAN_POINT('Ctrl Pts',(-0.24634740505191,-0.0263841469943832,
-0.0967343009784877));
#28675=CARTESIAN_POINT('Ctrl Pts',(-0.246149652364137,-0.000196946980918933,
-0.0975787219130166));
#28676=CARTESIAN_POINT('Ctrl Pts',(-0.246181916821291,-0.000205804393626753,
-0.104721278086982));
#28677=CARTESIAN_POINT('Ctrl Pts',(-0.246380499354541,-0.0251336934731506,
-0.103917198706219));
#28678=CARTESIAN_POINT('Ctrl Pts',(-0.242896536971094,-0.0500073764876101,
-0.103113119325457));
#28679=CARTESIAN_POINT('Ctrl Pts',(-0.235499587892452,-0.0736571948666213,
-0.102309039944694));
#28680=CARTESIAN_POINT('Ctrl Pts',(-0.211212101205851,-0.151310108644177,
-0.0996688883027656));
#28681=CARTESIAN_POINT('Ctrl Pts',(-0.144738622675513,-0.215768512051366,
-0.0970287366608371));
#28682=CARTESIAN_POINT('Ctrl Pts',(-0.0663750455930597,-0.237654800632327,
-0.0943885850189085));
#28683=CARTESIAN_POINT('Ctrl Pts',(0.0119885314893938,-0.259541089213289,
-0.0917484333769799));
#28684=CARTESIAN_POINT('Ctrl Pts',(0.102242207123963,-0.238855262968024,
-0.0891082817350513));
#28685=CARTESIAN_POINT('Ctrl Pts',(0.163251794345776,-0.185025147060926,
-0.0864681300931226));
#28686=CARTESIAN_POINT('Ctrl Pts',(0.224261381567592,-0.131195031153826,
-0.0838279784511939));
#28687=CARTESIAN_POINT('Ctrl Pts',(0.256026880376651,-0.0442206255848928,
-0.0811878268092653));
#28688=CARTESIAN_POINT('Ctrl Pts',(0.244071117874901,0.0362586807743849,
-0.0785476751673366));
#28689=CARTESIAN_POINT('Ctrl Pts',(0.232115355373152,0.11673798713366,-0.0759075235254081));
#28690=CARTESIAN_POINT('Ctrl Pts',(0.176438331560597,0.19072219428328,-0.0732673718834795));
#28691=CARTESIAN_POINT('Ctrl Pts',(0.102414890955883,0.224492068861293,
-0.0706272202415508));
#28692=CARTESIAN_POINT('Ctrl Pts',(0.0283914503511699,0.258261943439305,
-0.0679870685996222));
#28693=CARTESIAN_POINT('Ctrl Pts',(-0.0639784070457014,0.251817485445711,
-0.0653469169576935));
#28694=CARTESIAN_POINT('Ctrl Pts',(-0.132595160836082,0.208096147537468,
-0.0627067653157649));
#28695=CARTESIAN_POINT('Ctrl Pts',(-0.201211914626462,0.164374809629225,
-0.0600666136738363));
#28696=CARTESIAN_POINT('Ctrl Pts',(-0.24607556481035,0.0833765918063334,
-0.0574264620319078));
#28697=CARTESIAN_POINT('Ctrl Pts',(-0.246740958917921,0.00201664698560347,
-0.0547863103899792));
#28698=CARTESIAN_POINT('Ctrl Pts',(-0.246746422254512,0.00134862669725098,
-0.0547646329556469));
#28699=CARTESIAN_POINT('Ctrl Pts',(-0.246748905955546,0.000680582022990077,
-0.0547429555213145));
#28700=CARTESIAN_POINT('Ctrl Pts',(-0.246748421001242,1.25335797698571E-5,
-0.0547212780869822));
#28701=CARTESIAN_POINT('Origin',(0.,0.,-0.58));
#28702=CARTESIAN_POINT('',(-0.24635,-3.0169173896995E-17,0.));
#28703=CARTESIAN_POINT('',(-0.246160120813712,0.000192360259597545,-0.00472127808698222));
#28704=CARTESIAN_POINT('',(-0.24635,-3.0169173896995E-17,-0.58));
#28705=CARTESIAN_POINT('',(-0.235034375322676,0.0738049111962042,0.));
#28706=CARTESIAN_POINT('Origin',(0.,0.,0.));
#28707=CARTESIAN_POINT('Ctrl Pts',(-0.235034375322676,0.0738049111962042,
0.));
#28708=CARTESIAN_POINT('Ctrl Pts',(-0.21054802840921,0.151782557364509,
-0.0026401516419286));
#28709=CARTESIAN_POINT('Ctrl Pts',(-0.144434507356266,0.21595452844779,
-0.00528030328385723));
#28710=CARTESIAN_POINT('Ctrl Pts',(-0.0661699330088478,0.237693665813309,
-0.00792045492578582));
#28711=CARTESIAN_POINT('Ctrl Pts',(0.0120946413385708,0.259432803178828,
-0.0105606065677144));
#28712=CARTESIAN_POINT('Ctrl Pts',(0.102510268980464,0.238739106826586,
-0.0132007582096429));
#28713=CARTESIAN_POINT('Ctrl Pts',(0.163505372344248,0.184863010201967,
-0.0158409098515715));
#28714=CARTESIAN_POINT('Ctrl Pts',(0.224500475708032,0.130986913577347,
-0.0184810614935001));
#28715=CARTESIAN_POINT('Ctrl Pts',(0.256075054793706,0.0439284166803513,
-0.0211212131354288));
#28716=CARTESIAN_POINT('Ctrl Pts',(0.244005633311165,-0.0365487101329756,
-0.0237613647773574));
#28717=CARTESIAN_POINT('Ctrl Pts',(0.231936211828623,-0.117025836946305,
-0.0264015164192861));
#28718=CARTESIAN_POINT('Ctrl Pts',(0.176222789777864,-0.190921593675964,
-0.0290416680612148));
#28719=CARTESIAN_POINT('Ctrl Pts',(0.10217255517054,-0.224601453711439,
-0.0316818197031434));
#28720=CARTESIAN_POINT('Ctrl Pts',(0.0281223205632187,-0.258281313746913,
-0.034321971345072));
#28721=CARTESIAN_POINT('Ctrl Pts',(-0.064264726600667,-0.251745277088204,
-0.0369621229870006));
#28722=CARTESIAN_POINT('Ctrl Pts',(-0.132837988199004,-0.207949054077961,
-0.0396022746289292));
#28723=CARTESIAN_POINT('Ctrl Pts',(-0.201411249797341,-0.164152831067718,
-0.0422424262708578));
#28724=CARTESIAN_POINT('Ctrl Pts',(-0.246170725830129,-0.0830964217059404,
-0.0448825779127865));
#28725=CARTESIAN_POINT('Ctrl Pts',(-0.246740072055293,-0.001734289834587,
-0.0475227295547151));
#28726=CARTESIAN_POINT('Ctrl Pts',(-0.246744096955142,-0.00115911357481157,
-0.047541393674149));
#28727=CARTESIAN_POINT('Ctrl Pts',(-0.24674591343056,-0.000583922036396745,
-0.0475600577935829));
#28728=CARTESIAN_POINT('Ctrl Pts',(-0.246745528500925,-8.72836701185098E-6,
-0.0475787219130168));
#28729=CARTESIAN_POINT('Ctrl Pts',(-0.246748421001242,1.25335797698571E-5,
-0.0547212780869822));
#28730=CARTESIAN_POINT('Ctrl Pts',(-0.246689842097585,-0.0806827918530022,
-0.0521028038793859));
#28731=CARTESIAN_POINT('Ctrl Pts',(-0.203316033568085,-0.16143310963746,
-0.0494843296717896));
#28732=CARTESIAN_POINT('Ctrl Pts',(-0.135979279895863,-0.205901704836232,
-0.0468658554641934));
#28733=CARTESIAN_POINT('Ctrl Pts',(-0.0680850687349815,-0.25073844001877,
-0.0442257038222647));
#28734=CARTESIAN_POINT('Ctrl Pts',(0.0241704916180333,-0.258690238565275,
-0.041585552180336));
#28735=CARTESIAN_POINT('Ctrl Pts',(0.0987340617504916,-0.226135213676908,
-0.0389454005384073));
#28736=CARTESIAN_POINT('Ctrl Pts',(0.173297631882948,-0.193580188788542,
-0.0363052488964788));
#28737=CARTESIAN_POINT('Ctrl Pts',(0.230169211794848,-0.120518340465306,
-0.0336650972545502));
#28738=CARTESIAN_POINT('Ctrl Pts',(0.243442143508976,-0.0402441251670753,
-0.0310249456126216));
#28739=CARTESIAN_POINT('Ctrl Pts',(0.256715075223104,0.0400300901311557,
-0.028384793970693));
#28740=CARTESIAN_POINT('Ctrl Pts',(0.226389358739459,0.127516672404382,
-0.0257446423287643));
#28741=CARTESIAN_POINT('Ctrl Pts',(0.166261259011876,0.182334672033693,
-0.0231044906868356));
#28742=CARTESIAN_POINT('Ctrl Pts',(0.106133159284294,0.237152671663005,
-0.020464339044907));
#28743=CARTESIAN_POINT('Ctrl Pts',(0.0162026763127736,0.259302088648401,
-0.0178241874029785));
#28744=CARTESIAN_POINT('Ctrl Pts',(-0.0624958806646685,0.238703388389264,
-0.0151840357610499));
#28745=CARTESIAN_POINT('Ctrl Pts',(-0.141194437642113,0.218104688130128,
-0.0125438841191213));
#28746=CARTESIAN_POINT('Ctrl Pts',(-0.208661068625478,0.154757870626456,
-0.00990373247719252));
#28747=CARTESIAN_POINT('Ctrl Pts',(-0.234238261452687,0.0775047438993852,
-0.00726358083526382));
#28748=CARTESIAN_POINT('Ctrl Pts',(-0.242448013067616,0.052708082819708,
-0.00641614658583661));
#28749=CARTESIAN_POINT('Ctrl Pts',(-0.246341989476513,0.0264786857761341,
-0.00556871233640941));
#28750=CARTESIAN_POINT('Ctrl Pts',(-0.246160120813712,0.000192360259597545,
-0.00472127808698222));
#28751=CARTESIAN_POINT('Origin',(0.,0.,-1.25608093797092));
#28752=CARTESIAN_POINT('',(-0.218124649763706,-7.71593311516547E-6,-0.0310809379709236));
#28753=CARTESIAN_POINT('',(-0.217607145566089,0.000170047718830516,-0.0212190620290759));
#28754=CARTESIAN_POINT('',(-0.217775,1.66341393608259E-15,-1.25608093797092));
#28755=CARTESIAN_POINT('',(0.157411390703589,0.150985252349406,2.08166817117217E-17));
#28756=CARTESIAN_POINT('Ctrl Pts',(-0.218124649763706,-7.71593311514433E-6,
-0.0310809379709236));
#28757=CARTESIAN_POINT('Ctrl Pts',(-0.218124990044004,-0.0005161908726374,
-0.0310622738514896));
#28758=CARTESIAN_POINT('Ctrl Pts',(-0.21789623761169,-0.0729512274990299,
-0.0284034580901269));
#28759=CARTESIAN_POINT('Ctrl Pts',(-0.138481185433633,-0.216766561130641,
-0.0231044906868355));
#28760=CARTESIAN_POINT('Ctrl Pts',(0.106531063757949,-0.234100257700769,
-0.0151840357610497));
#28761=CARTESIAN_POINT('Ctrl Pts',(0.250199565624991,-0.0435448713522292,
-0.0074825388654379));
#28762=CARTESIAN_POINT('Ctrl Pts',(0.202824236587796,0.103068069205317,
-0.00242119361175455));
#28763=CARTESIAN_POINT('Ctrl Pts',(0.157411390703589,0.150985252349406,
2.64816380629584E-17));
#28764=CARTESIAN_POINT('',(0.193653104151514,-0.0996214127458699,0.));
#28765=CARTESIAN_POINT('Origin',(0.,0.,0.));
#28766=CARTESIAN_POINT('Ctrl Pts',(-0.217607145566089,0.000170047718830547,
-0.0212190620290759));
#28767=CARTESIAN_POINT('Ctrl Pts',(-0.21726703576361,-0.0489876072703885,
-0.0194263446365745));
#28768=CARTESIAN_POINT('Ctrl Pts',(-0.176554978527624,-0.171097090088319,
-0.0149934756021445));
#28769=CARTESIAN_POINT('Ctrl Pts',(0.0261231005236458,-0.255800095598605,
-0.00792045492578602));
#28770=CARTESIAN_POINT('Ctrl Pts',(0.160601584503721,-0.163869943260562,
-0.0026401516419286));
#28771=CARTESIAN_POINT('Ctrl Pts',(0.193653104151514,-0.0996214127458699,
0.));
#28772=CARTESIAN_POINT('Origin',(0.,0.,-1.25608093797092));
#28773=CARTESIAN_POINT('',(-0.217597891388674,-0.00017410241024964,-0.0810809379709236));
#28774=CARTESIAN_POINT('',(-0.218127206752773,1.10797659262985E-5,-0.071219062029076));
#28775=CARTESIAN_POINT('',(-0.217775,1.66341393608259E-15,-1.25608093797092));
#28776=CARTESIAN_POINT('Ctrl Pts',(-0.217597891388674,-0.000174102410249656,
-0.0810809379709236));
#28777=CARTESIAN_POINT('Ctrl Pts',(-0.217772706049037,-0.023323757303425,
-0.0802365170363945));
#28778=CARTESIAN_POINT('Ctrl Pts',(-0.203726648457932,-0.118646141873473,
-0.0767519444599368));
#28779=CARTESIAN_POINT('Ctrl Pts',(-0.0654119898536204,-0.248746182667544,
-0.0706272202415509));
#28780=CARTESIAN_POINT('Ctrl Pts',(0.173081747182517,-0.190252584181875,
-0.0627067653157647));
#28781=CARTESIAN_POINT('Ctrl Pts',(0.253804655411944,0.0416584463135328,
-0.0547863103899791));
#28782=CARTESIAN_POINT('Ctrl Pts',(0.103185600053364,0.235600191315231,
-0.0468658554641932));
#28783=CARTESIAN_POINT('Ctrl Pts',(-0.140924429342837,0.214830415357785,
-0.0389640646578413));
#28784=CARTESIAN_POINT('Ctrl Pts',(-0.218076855354893,0.0714106391716104,
-0.0337024254934182));
#28785=CARTESIAN_POINT('Ctrl Pts',(-0.218124649763706,-7.71593311514433E-6,
-0.0310809379709236));
#28786=CARTESIAN_POINT('Ctrl Pts',(-0.218127206752773,1.10797659263097E-5,
-0.071219062029076));
#28787=CARTESIAN_POINT('Ctrl Pts',(-0.218075422621483,-0.0713241120186178,
-0.0686005878214797));
#28788=CARTESIAN_POINT('Ctrl Pts',(-0.141072539660443,-0.214682684397483,
-0.0633419619719547));
#28789=CARTESIAN_POINT('Ctrl Pts',(0.102921386109171,-0.235713292600032,
-0.055443184480501));
#28790=CARTESIAN_POINT('Ctrl Pts',(0.253745924148315,-0.0419518472751756,
-0.0475227295547153));
#28791=CARTESIAN_POINT('Ctrl Pts',(0.173321533153074,0.190064273543398,
-0.0396022746289292));
#28792=CARTESIAN_POINT('Ctrl Pts',(-0.0651758599354944,0.248804958958394,
-0.0316818197031436));
#28793=CARTESIAN_POINT('Ctrl Pts',(-0.203601252094894,0.118832438807541,
-0.025554082169859));
#28794=CARTESIAN_POINT('Ctrl Pts',(-0.21776791864521,0.0234073302005182,
-0.0220664962785031));
#28795=CARTESIAN_POINT('Ctrl Pts',(-0.217607145566089,0.000170047718830547,
-0.0212190620290759));
#28796=CARTESIAN_POINT('Origin',(0.,0.,-1.25608093797092));
#28797=CARTESIAN_POINT('',(-0.217520312610843,0.000140789959117709,-0.131080937970923));
#28798=CARTESIAN_POINT('',(-0.21762641337835,-0.000181932420623115,-0.121219062029076));
#28799=CARTESIAN_POINT('',(-0.217775,1.66341393608259E-15,-1.25608093797092));
#28800=CARTESIAN_POINT('Ctrl Pts',(-0.217520312610843,0.000140789959117728,
-0.131080937970923));
#28801=CARTESIAN_POINT('Ctrl Pts',(-0.217247281722338,-0.0456880330405798,
-0.129410760221299));
#28802=CARTESIAN_POINT('Ctrl Pts',(-0.180717894981605,-0.164359326083748,
-0.125100430829747));
#28803=CARTESIAN_POINT('Ctrl Pts',(0.0139231655990339,-0.256825521944582,
-0.118149949796266));
#28804=CARTESIAN_POINT('Ctrl Pts',(0.223036130664036,-0.128094072175867,
-0.11022949487048));
#28805=CARTESIAN_POINT('Ctrl Pts',(0.228847010841678,0.117397719925839,
-0.102309039944694));
#28806=CARTESIAN_POINT('Ctrl Pts',(0.0260592703673014,0.255879147195341,
-0.0943885850189083));
#28807=CARTESIAN_POINT('Ctrl Pts',(-0.176330078465526,0.171223727000115,
-0.0873125510276516));
#28808=CARTESIAN_POINT('Ctrl Pts',(-0.217226133606649,0.0490555465213744,
-0.0828766686783232));
#28809=CARTESIAN_POINT('Ctrl Pts',(-0.217597891388674,-0.000174102410249656,
-0.0810809379709236));
#28810=CARTESIAN_POINT('Ctrl Pts',(-0.21762641337835,-0.000181932420623089,
-0.121219062029076));
#28811=CARTESIAN_POINT('Ctrl Pts',(-0.217801961627503,-0.0222183482691874,
-0.120414982648313));
#28812=CARTESIAN_POINT('Ctrl Pts',(-0.204609608685256,-0.116404900586581,
-0.116970751625622));
#28813=CARTESIAN_POINT('Ctrl Pts',(-0.0691868957427056,-0.24772241328998,
-0.110886368961002));
#28814=CARTESIAN_POINT('Ctrl Pts',(0.170167610585507,-0.192863199035107,
-0.102965914035216));
#28815=CARTESIAN_POINT('Ctrl Pts',(0.254410332361144,0.0377946191841849,
-0.0950454591094304));
#28816=CARTESIAN_POINT('Ctrl Pts',(0.106753780372761,0.234002178088288,
-0.0871250041836445));
#28817=CARTESIAN_POINT('Ctrl Pts',(-0.138212881221763,0.216911349922406,
-0.0792045492578586));
#28818=CARTESIAN_POINT('Ctrl Pts',(-0.217858031003544,0.0731175399198877,
-0.0739025685396692));
#28819=CARTESIAN_POINT('Ctrl Pts',(-0.218127635455527,0.000601638928588284,
-0.0712407394634083));
#28820=CARTESIAN_POINT('Ctrl Pts',(-0.218127206752773,1.10797659263097E-5,
-0.071219062029076));
#28821=CARTESIAN_POINT('Origin',(0.,0.,-1.25608093797092));
#28822=CARTESIAN_POINT('',(-0.218099944255961,7.07777948932365E-5,-0.181080937970924));
#28823=CARTESIAN_POINT('',(-0.217499459018025,0.000127504564585532,-0.171219062029076));
#28824=CARTESIAN_POINT('',(-0.217775,1.66341393608259E-15,-1.25608093797092));
#28825=CARTESIAN_POINT('Ctrl Pts',(-0.218099944255961,7.07777948932352E-5,
-0.181080937970924));
#28826=CARTESIAN_POINT('Ctrl Pts',(-0.217810429495954,-0.0679491065147507,
-0.178585003406205));
#28827=CARTESIAN_POINT('Ctrl Pts',(-0.147066455741474,-0.20843871206212,
-0.173448917199557));
#28828=CARTESIAN_POINT('Ctrl Pts',(0.0919194261743976,-0.240216610307221,
-0.165672679350981));
#28829=CARTESIAN_POINT('Ctrl Pts',(0.25155106383961,-0.0536214810419249,
-0.157752224425195));
#28830=CARTESIAN_POINT('Ctrl Pts',(0.181888736963096,0.181850729131537,
-0.149831769499409));
#28831=CARTESIAN_POINT('Ctrl Pts',(-0.0535689079525661,0.251562264853035,
-0.141911314573623));
#28832=CARTESIAN_POINT('Ctrl Pts',(-0.200843250451035,0.125622751888632,
-0.135661037397461));
#28833=CARTESIAN_POINT('Ctrl Pts',(-0.217678878268721,0.0267563773328428,
-0.132050911863228));
#28834=CARTESIAN_POINT('Ctrl Pts',(-0.217520312610843,0.000140789959117728,
-0.131080937970923));
#28835=CARTESIAN_POINT('Ctrl Pts',(-0.217499459018025,0.000127504564585532,
-0.171219062029076));
#28836=CARTESIAN_POINT('Ctrl Pts',(-0.217259599358021,-0.0446051280446579,
-0.169589225833218));
#28837=CARTESIAN_POINT('Ctrl Pts',(-0.182075110663368,-0.162145796313866,
-0.165319237995432));
#28838=CARTESIAN_POINT('Ctrl Pts',(0.0100158074287402,-0.257007551691304,
-0.158409098515717));
#28839=CARTESIAN_POINT('Ctrl Pts',(0.221062284030839,-0.131471158330418,
-0.150488643589931));
#28840=CARTESIAN_POINT('Ctrl Pts',(0.230605935914093,0.113903893563196,
-0.142568188664146));
#28841=CARTESIAN_POINT('Ctrl Pts',(0.0299475598214531,0.255453212845186,
-0.13464773373836));
#28842=CARTESIAN_POINT('Ctrl Pts',(-0.174866704728409,0.173420540348032,
-0.127531358193336));
#28843=CARTESIAN_POINT('Ctrl Pts',(-0.217225558340306,0.0501370445897034,
-0.123055134290242));
#28844=CARTESIAN_POINT('Ctrl Pts',(-0.21762641337835,-0.000181932420623089,
-0.121219062029076));
#28845=CARTESIAN_POINT('Origin',(0.,0.,-1.25608093797092));
#28846=CARTESIAN_POINT('',(-0.217720465391163,-0.00019571213919499,-0.231080937970923));
#28847=CARTESIAN_POINT('',(-0.218083107449943,8.90825909709205E-5,-0.221219062029075));
#28848=CARTESIAN_POINT('',(-0.217775,1.66341393608259E-15,-1.25608093797092));
#28849=CARTESIAN_POINT('Ctrl Pts',(-0.217720465391163,-0.000195712139194972,
-0.231080937970923));
#28850=CARTESIAN_POINT('Ctrl Pts',(-0.217886022198555,-0.01885336084795,
-0.230399398233038));
#28851=CARTESIAN_POINT('Ctrl Pts',(-0.207164530811011,-0.109599730208546,
-0.227077706853224));
#28852=CARTESIAN_POINT('Ctrl Pts',(-0.0805528101499051,-0.244263066255845,
-0.221115863831482));
#28853=CARTESIAN_POINT('Ctrl Pts',(0.161079512847755,-0.200515813094597,
-0.213195408905696));
#28854=CARTESIAN_POINT('Ctrl Pts',(0.255884550354012,0.0260057235181914,
-0.20527495397991));
#28855=CARTESIAN_POINT('Ctrl Pts',(0.117445562765472,0.228822508812962,
-0.197354499054125));
#28856=CARTESIAN_POINT('Ctrl Pts',(-0.128047468266331,0.223062875957976,
-0.189434044128339));
#28857=CARTESIAN_POINT('Ctrl Pts',(-0.216242317834423,0.079865114777898,
-0.184009523767272));
#28858=CARTESIAN_POINT('Ctrl Pts',(-0.218116672648238,0.00400102061694045,
-0.181225155048133));
#28859=CARTESIAN_POINT('Ctrl Pts',(-0.218099944255961,7.07777948932352E-5,
-0.181080937970924));
#28860=CARTESIAN_POINT('Ctrl Pts',(-0.218083107449943,8.90825909709344E-5,
-0.221219062029075));
#28861=CARTESIAN_POINT('Ctrl Pts',(-0.217735478436945,-0.0668451408398962,
-0.218763469018123));
#28862=CARTESIAN_POINT('Ctrl Pts',(-0.148982183502457,-0.206361735170698,
-0.213667724365242));
#28863=CARTESIAN_POINT('Ctrl Pts',(0.0882556230412838,-0.241586718983118,
-0.205931828070432));
#28864=CARTESIAN_POINT('Ctrl Pts',(0.250706501180205,-0.0574408224581984,
-0.198011373144647));
#28865=CARTESIAN_POINT('Ctrl Pts',(0.184633252234903,0.179063563844805,
-0.190090918218861));
#28866=CARTESIAN_POINT('Ctrl Pts',(-0.0497369991668516,0.252347832796275,
-0.182170463293075));
#28867=CARTESIAN_POINT('Ctrl Pts',(-0.199872383158113,0.127864301170981,
-0.175879844563147));
#28868=CARTESIAN_POINT('Ctrl Pts',(-0.217648145076176,0.0278567142749893,
-0.172229377475147));
#28869=CARTESIAN_POINT('Ctrl Pts',(-0.217499459018025,0.000127504564585532,
-0.171219062029076));
#28870=CARTESIAN_POINT('Origin',(0.,0.,-1.25608093797092));
#28871=CARTESIAN_POINT('',(-0.217450356241808,8.11937875190503E-5,-0.281080937970923));
#28872=CARTESIAN_POINT('',(-0.217753140028605,-0.000196789279391762,-0.271219062029075));
#28873=CARTESIAN_POINT('',(-0.217775,1.66341393608259E-15,-1.25608093797092));
#28874=CARTESIAN_POINT('Ctrl Pts',(-0.217450356241808,8.11937875190537E-5,
-0.281080937970923));
#28875=CARTESIAN_POINT('Ctrl Pts',(-0.217310991296762,-0.0413116087876461,
-0.279573641417943));
#28876=CARTESIAN_POINT('Ctrl Pts',(-0.186043658368974,-0.155402323209727,
-0.275426193223034));
#28877=CARTESIAN_POINT('Ctrl Pts',(-0.00186346654402013,-0.257195894705197,
-0.268638593386197));
#28878=CARTESIAN_POINT('Ctrl Pts',(0.214755114225321,-0.141539541029435,
-0.260718138460412));
#28879=CARTESIAN_POINT('Ctrl Pts',(0.235619996010104,0.103133012372812,
-0.252797683534625));
#28880=CARTESIAN_POINT('Ctrl Pts',(0.0417124103716506,0.25379770602124,
-0.24487722860884));
#28881=CARTESIAN_POINT('Ctrl Pts',(-0.170259828869626,0.180062686173349,
-0.237638313420939));
#28882=CARTESIAN_POINT('Ctrl Pts',(-0.217244687508043,0.0534227209925802,
-0.233039549874966));
#28883=CARTESIAN_POINT('Ctrl Pts',(-0.217720465391163,-0.000195712139194972,
-0.231080937970923));
#28884=CARTESIAN_POINT('Ctrl Pts',(-0.217753140028605,-0.000196789279391723,
-0.271219062029075));
#28885=CARTESIAN_POINT('Ctrl Pts',(-0.217911809312456,-0.0177433382782513,
-0.270577863844957));
#28886=CARTESIAN_POINT('Ctrl Pts',(-0.207964564278322,-0.107360671848747,
-0.267296514018909));
#28887=CARTESIAN_POINT('Ctrl Pts',(-0.084258201720026,-0.243009780113768,
-0.261375012550933));
#28888=CARTESIAN_POINT('Ctrl Pts',(0.158011472529912,-0.202942288192858,
-0.253454557625148));
#28889=CARTESIAN_POINT('Ctrl Pts',(0.256250443060382,0.0221112690783347,
-0.245534102699361));
#28890=CARTESIAN_POINT('Ctrl Pts',(0.120911869802921,0.227009950283883,
-0.237613647773576));
#28891=CARTESIAN_POINT('Ctrl Pts',(-0.124640357031449,0.224984397651718,
-0.22969319284779));
#28892=CARTESIAN_POINT('Ctrl Pts',(-0.215674746029958,0.0820896034994043,
-0.224228330932957));
#28893=CARTESIAN_POINT('Ctrl Pts',(-0.218109234717141,0.00511975688706352,
-0.221403620660052));
#28894=CARTESIAN_POINT('Ctrl Pts',(-0.218083107449943,8.90825909709344E-5,
-0.221219062029075));
#28895=CARTESIAN_POINT('Origin',(0.,0.,-1.25608093797092));
#28896=CARTESIAN_POINT('',(-0.218013928034523,0.000137760041710202,-0.331080937970923));
#28897=CARTESIAN_POINT('',(-0.217439216836811,6.44253989956767E-5,-0.321219062029076));
#28898=CARTESIAN_POINT('',(-0.217775,1.66341393608259E-15,-1.25608093797092));
#28899=CARTESIAN_POINT('Ctrl Pts',(-0.218013928034523,0.000137760041710215,
-0.331080937970923));
#28900=CARTESIAN_POINT('Ctrl Pts',(-0.217543145477283,-0.0635095455130215,
-0.328747884602848));
#28901=CARTESIAN_POINT('Ctrl Pts',(-0.154624849848435,-0.199992517491552,
-0.323774679592845));
#28902=CARTESIAN_POINT('Ctrl Pts',(0.0770050110794473,-0.245404623080814,
-0.316161322940912));
#28903=CARTESIAN_POINT('Ctrl Pts',(0.247786424439417,-0.0689571506394352,
-0.308240868015127));
#28904=CARTESIAN_POINT('Ctrl Pts',(0.192705420891506,0.170346181406604,
-0.300320413089341));
#28905=CARTESIAN_POINT('Ctrl Pts',(-0.038030533133535,0.254375469159979,
-0.292399958163555));
#28906=CARTESIAN_POINT('Ctrl Pts',(-0.196787847617761,0.1346707203534,-0.285986799790749));
#28907=CARTESIAN_POINT('Ctrl Pts',(-0.217555100253134,0.0311912278086411,
-0.282213793059872));
#28908=CARTESIAN_POINT('Ctrl Pts',(-0.217450356241808,8.11937875190537E-5,
-0.281080937970923));
#28909=CARTESIAN_POINT('Ctrl Pts',(-0.217439216836811,6.44253989956801E-5,
-0.321219062029076));
#28910=CARTESIAN_POINT('Ctrl Pts',(-0.217331911137438,-0.0402256889947239,
-0.319752107029862));
#28911=CARTESIAN_POINT('Ctrl Pts',(-0.187300136972098,-0.153176608816098,
-0.315645000388719));
#28912=CARTESIAN_POINT('Ctrl Pts',(-0.00577464009454566,-0.257137806088364,
-0.308897742105649));
#28913=CARTESIAN_POINT('Ctrl Pts',(0.212577765931518,-0.144789126731672,
-0.300977287179862));
#28914=CARTESIAN_POINT('Ctrl Pts',(0.237161170678426,0.0995378164850663,
-0.293056832254077));
#28915=CARTESIAN_POINT('Ctrl Pts',(0.0455672956274394,0.253133994867042,
-0.285136377328291));
#28916=CARTESIAN_POINT('Ctrl Pts',(-0.168689180999164,0.182238236202396,
-0.277857120586624));
#28917=CARTESIAN_POINT('Ctrl Pts',(-0.217258484052562,0.0545050730506043,
-0.273218015486885));
#28918=CARTESIAN_POINT('Ctrl Pts',(-0.217753140028605,-0.000196789279391723,
-0.271219062029075));
#28919=CARTESIAN_POINT('Origin',(0.,0.,-1.25608093797092));
#28920=CARTESIAN_POINT('',(-0.217853960473376,-0.000189083574295208,-0.381080937970923));
#28921=CARTESIAN_POINT('',(-0.217986410727679,0.000151022126422644,-0.371219062029075));
#28922=CARTESIAN_POINT('',(-0.217775,1.66341393608259E-15,-1.25608093797092));
#28923=CARTESIAN_POINT('Ctrl Pts',(-0.217853960473376,-0.000189083574295203,
-0.381080937970923));
#28924=CARTESIAN_POINT('Ctrl Pts',(-0.217983094335092,-0.0143654608404639,
-0.380562279429682));
#28925=CARTESIAN_POINT('Ctrl Pts',(-0.210272990147377,-0.100564696279621,
-0.377403469246512));
#28926=CARTESIAN_POINT('Ctrl Pts',(-0.0953904860153474,-0.238859489948667,
-0.371604507421413));
#28927=CARTESIAN_POINT('Ctrl Pts',(0.148471039289085,-0.210022739847858,
-0.363684052495628));
#28928=CARTESIAN_POINT('Ctrl Pts',(0.256998161788665,0.0102540527612222,
-0.355763597569842));
#28929=CARTESIAN_POINT('Ctrl Pts',(0.13126617952173,0.221184065598206,-0.347843142644056));
#28930=CARTESIAN_POINT('Ctrl Pts',(-0.11411762238027,0.230500258184359,
-0.33992268771827));
#28931=CARTESIAN_POINT('Ctrl Pts',(-0.213840835196708,0.0888553987055005,
-0.334335286160559));
#28932=CARTESIAN_POINT('Ctrl Pts',(-0.21807589683158,0.00851561283271852,
-0.331388036244777));
#28933=CARTESIAN_POINT('Ctrl Pts',(-0.218013928034523,0.000137760041710215,
-0.331080937970923));
#28934=CARTESIAN_POINT('Ctrl Pts',(-0.217986410727679,0.000151022126422642,
-0.371219062029075));
#28935=CARTESIAN_POINT('Ctrl Pts',(-0.217490935156433,-0.0624164103471532,
-0.368926350214767));
#28936=CARTESIAN_POINT('Ctrl Pts',(-0.156424859230848,-0.197877144388145,
-0.36399348675853));
#28937=CARTESIAN_POINT('Ctrl Pts',(0.0732640345114102,-0.246547316017172,
-0.356420471660364));
#28938=CARTESIAN_POINT('Ctrl Pts',(0.246709075468843,-0.0727174660550607,
-0.348500016734578));
#28939=CARTESIAN_POINT('Ctrl Pts',(0.195273725240327,0.167395848272668,
-0.340579561808792));
#28940=CARTESIAN_POINT('Ctrl Pts',(-0.0341576376477591,0.254924407577,-0.332659106883006));
#28941=CARTESIAN_POINT('Ctrl Pts',(-0.195727025771613,0.136910137110939,
-0.326205606956434));
#28942=CARTESIAN_POINT('Ctrl Pts',(-0.217525034524685,0.0322864274144955,
-0.322392258671791));
#28943=CARTESIAN_POINT('Ctrl Pts',(-0.217439216836811,6.44253989956801E-5,
-0.321219062029076));
#28944=CARTESIAN_POINT('Origin',(0.,0.,-1.25608093797092));
#28945=CARTESIAN_POINT('',(-0.217421696185068,1.08647192597108E-5,-0.431080937970923));
#28946=CARTESIAN_POINT('',(-0.217886707632715,-0.000182918697169548,-0.421219062029076));
#28947=CARTESIAN_POINT('',(-0.217775,1.66341393608259E-15,-1.25608093797092));
#28948=CARTESIAN_POINT('Ctrl Pts',(-0.217421696185068,1.0864719259724E-5,
-0.431080937970923));
#28949=CARTESIAN_POINT('Ctrl Pts',(-0.217405187502425,-0.0369211171181637,
-0.429736522614587));
#28950=CARTESIAN_POINT('Ctrl Pts',(-0.190967954382265,-0.146401997414083,
-0.425751955616322));
#28951=CARTESIAN_POINT('Ctrl Pts',(-0.0176430849829593,-0.256596808852072,
-0.419127236976129));
#28952=CARTESIAN_POINT('Ctrl Pts',(0.205664628051519,-0.154451486005192,
-0.411206782050343));
#28953=CARTESIAN_POINT('Ctrl Pts',(0.241504807022057,0.0884795397028073,
-0.403286327124557));
#28954=CARTESIAN_POINT('Ctrl Pts',(0.0572083924230321,0.250759647066977,
-0.395365872198771));
#28955=CARTESIAN_POINT('Ctrl Pts',(-0.163751546468412,0.188808241753342,
-0.387964075814226));
#28956=CARTESIAN_POINT('Ctrl Pts',(-0.217325758246069,0.0577972102423321,
-0.38320243107161));
#28957=CARTESIAN_POINT('Ctrl Pts',(-0.217853960473376,-0.000189083574295203,
-0.381080937970923));
#28958=CARTESIAN_POINT('Ctrl Pts',(-0.217886707632715,-0.000182918697169543,
-0.421219062029076));
#28959=CARTESIAN_POINT('Ctrl Pts',(-0.218003945711644,-0.0132515775492716,
-0.420740745041601));
#28960=CARTESIAN_POINT('Ctrl Pts',(-0.210993560192625,-0.0983293864088883,
-0.417622276412197));
#28961=CARTESIAN_POINT('Ctrl Pts',(-0.0990119847176032,-0.237381180110053,
-0.411863656140865));
#28962=CARTESIAN_POINT('Ctrl Pts',(0.145259877725951,-0.212256367893173,
-0.403943201215079));
#28963=CARTESIAN_POINT('Ctrl Pts',(0.25712437710612,0.00634448468750714,
-0.396022746289293));
#28964=CARTESIAN_POINT('Ctrl Pts',(0.134614723864691,0.219162209121448,
-0.388102291363507));
#28965=CARTESIAN_POINT('Ctrl Pts',(-0.11059901597976,0.232209077024282,
-0.380181836437722));
#28966=CARTESIAN_POINT('Ctrl Pts',(-0.213200284022019,0.0910855532474006,
-0.374554093326244));
#28967=CARTESIAN_POINT('Ctrl Pts',(-0.218061495588318,0.00963255304434301,
-0.371566501856695));
#28968=CARTESIAN_POINT('Ctrl Pts',(-0.217986410727679,0.000151022126422642,
-0.371219062029075));
#28969=CARTESIAN_POINT('Origin',(0.,0.,-1.25608093797092));
#28970=CARTESIAN_POINT('',(-0.217893402471771,0.000181423312113251,-0.481080937970923));
#28971=CARTESIAN_POINT('',(-0.217421408434359,-7.14500207714408E-6,-0.471219062029076));
#28972=CARTESIAN_POINT('',(-0.217775,1.66341393608259E-15,-1.25608093797092));
#28973=CARTESIAN_POINT('Ctrl Pts',(-0.217893402471771,0.000181423312113252,
-0.481080937970923));
#28974=CARTESIAN_POINT('Ctrl Pts',(-0.217363839693254,-0.0591076871415457,
-0.478910765799492));
#28975=CARTESIAN_POINT('Ctrl Pts',(-0.161719648021016,-0.191400681792459,
-0.474100441986132));
#28976=CARTESIAN_POINT('Ctrl Pts',(0.0618003361169582,-0.249667617476944,
-0.466649966530844));
#28977=CARTESIAN_POINT('Ctrl Pts',(0.243087789097186,-0.0840328956577408,
-0.458729511605058));
#28978=CARTESIAN_POINT('Ctrl Pts',(0.202795727822344,0.158199537097262,
-0.450809056679272));
#28979=CARTESIAN_POINT('Ctrl Pts',(-0.0223488060129853,0.256229841413087,
-0.442888601753486));
#28980=CARTESIAN_POINT('Ctrl Pts',(-0.192363820390413,0.143705936117005,
-0.436312562184037));
#28981=CARTESIAN_POINT('Ctrl Pts',(-0.217437607115442,0.0356056001855403,
-0.432376674256515));
#28982=CARTESIAN_POINT('Ctrl Pts',(-0.217421696185068,1.0864719259724E-5,
-0.431080937970923));
#28983=CARTESIAN_POINT('Ctrl Pts',(-0.217421408434359,-7.14500207711632E-6,
-0.471219062029076));
#28984=CARTESIAN_POINT('Ctrl Pts',(-0.217431938551127,-0.035831033129075,
-0.469914988226506));
#28985=CARTESIAN_POINT('Ctrl Pts',(-0.19212717751519,-0.144167867511391,
-0.465970762782007));
#28986=CARTESIAN_POINT('Ctrl Pts',(-0.0215433225451699,-0.256298815919768,
-0.45938638569558));
#28987=CARTESIAN_POINT('Ctrl Pts',(0.203291968690357,-0.157561331722472,
-0.451465930769794));
#28988=CARTESIAN_POINT('Ctrl Pts',(0.242822453618414,0.0847965436022809,
-0.443545475844009));
#28989=CARTESIAN_POINT('Ctrl Pts',(0.0610152830318996,0.24986062719984,
-0.435625020918222));
#28990=CARTESIAN_POINT('Ctrl Pts',(-0.162070523658039,0.19095741053108,
-0.428182882979912));
#28991=CARTESIAN_POINT('Ctrl Pts',(-0.217356830274212,0.0588830988884751,
-0.423380896683529));
#28992=CARTESIAN_POINT('Ctrl Pts',(-0.217886707632715,-0.000182918697169543,
-0.421219062029076));
#28993=CARTESIAN_POINT('Origin',(0.,0.,-1.25608093797092));
#28994=CARTESIAN_POINT('',(-0.217980498315397,-0.00015357182946072,-0.531080937970923));
#28995=CARTESIAN_POINT('',(-0.217860768206988,0.000187955723751763,-0.521219062029076));
#28996=CARTESIAN_POINT('',(-0.217775,1.66341393608259E-15,-1.25608093797092));
#28997=CARTESIAN_POINT('Ctrl Pts',(-0.217980498315397,-0.000153571829460759,
-0.531080937970923));
#28998=CARTESIAN_POINT('Ctrl Pts',(-0.218058321777369,-0.00986332003771939,
-0.530725160626326));
#28999=CARTESIAN_POINT('Ctrl Pts',(-0.213065599226933,-0.0915466328813675,
-0.527729231639799));
#29000=CARTESIAN_POINT('Ctrl Pts',(-0.109868600748205,-0.232555566113592,
-0.522093151011346));
#29001=CARTESIAN_POINT('Ctrl Pts',(0.135302924854754,-0.21873801518376,
-0.514172696085558));
#29002=CARTESIAN_POINT('Ctrl Pts',(0.257143054512441,-0.0055362692125341,
-0.506252241159774));
#29003=CARTESIAN_POINT('Ctrl Pts',(0.144592006708923,0.212711899894362,
-0.498331786233987));
#29004=CARTESIAN_POINT('Ctrl Pts',(-0.0997576260038526,0.237068801858992,
-0.490411331308202));
#29005=CARTESIAN_POINT('Ctrl Pts',(-0.211140091175798,0.0978675476797122,
-0.484661048553847));
#29006=CARTESIAN_POINT('Ctrl Pts',(-0.218008086291571,0.013021263903609,
-0.481550917441421));
#29007=CARTESIAN_POINT('Ctrl Pts',(-0.217893402471771,0.000181423312113252,
-0.481080937970923));
#29008=CARTESIAN_POINT('Ctrl Pts',(-0.217860768206988,0.000187955723751776,
-0.521219062029076));
#29009=CARTESIAN_POINT('Ctrl Pts',(-0.217331798266099,-0.0580215318518826,
-0.519089231411411));
#29010=CARTESIAN_POINT('Ctrl Pts',(-0.163406389880727,-0.189253002387909,
-0.514319249151818));
#29011=CARTESIAN_POINT('Ctrl Pts',(0.0579962873891273,-0.250578587347838,
-0.506909115250295));
#29012=CARTESIAN_POINT('Ctrl Pts',(0.241781714379012,-0.087720011286514,
-0.49898866032451));
#29013=CARTESIAN_POINT('Ctrl Pts',(0.205178141054117,0.155097157361885,
-0.491068205398723));
#29014=CARTESIAN_POINT('Ctrl Pts',(-0.0184495234412028,0.256540080441542,
-0.483147750472938));
#29015=CARTESIAN_POINT('Ctrl Pts',(-0.191209471905011,0.145940397476656,
-0.476531369349722));
#29016=CARTESIAN_POINT('Ctrl Pts',(-0.217410619891846,0.0366959180851669,
-0.472555139868434));
#29017=CARTESIAN_POINT('Ctrl Pts',(-0.217421408434359,-7.14500207711632E-6,
-0.471219062029076));
#29018=CARTESIAN_POINT('Origin',(0.,0.,-1.25608093797092));
#29019=CARTESIAN_POINT('',(-0.217437245756766,-6.08897400841611E-5,-0.581080937970923));
#29020=CARTESIAN_POINT('',(-0.218008398413668,-0.000140623921195487,-0.571219062029076));
#29021=CARTESIAN_POINT('',(-0.217775,1.66341393608259E-15,-1.25608093797092));
#29022=CARTESIAN_POINT('Ctrl Pts',(-0.217437245756766,-6.08897400841621E-5,
-0.581080937970923));
#29023=CARTESIAN_POINT('Ctrl Pts',(-0.217518887675132,-0.0325126204013041,
-0.579899403811231));
#29024=CARTESIAN_POINT('Ctrl Pts',(-0.195504947923748,-0.13737285598521,
-0.57607771800961));
#29025=CARTESIAN_POINT('Ctrl Pts',(-0.033356200274203,-0.255030517123049,
-0.569615880566061));
#29026=CARTESIAN_POINT('Ctrl Pts',(0.195798917752269,-0.166781247650396,
-0.561695425640274));
#29027=CARTESIAN_POINT('Ctrl Pts',(0.246479299353905,0.0734925557508373,
-0.553774970714489));
#29028=CARTESIAN_POINT('Ctrl Pts',(0.0724887354193506,0.246776384603724,
-0.545854515788701));
#29029=CARTESIAN_POINT('Ctrl Pts',(-0.156793344004563,0.197438880298673,
-0.538289838207515));
#29030=CARTESIAN_POINT('Ctrl Pts',(-0.217480809622574,0.0621907555351431,
-0.533365312268254));
#29031=CARTESIAN_POINT('Ctrl Pts',(-0.217980498315397,-0.000153571829460759,
-0.531080937970923));
#29032=CARTESIAN_POINT('Ctrl Pts',(-0.218008398413668,-0.000140623921195505,
-0.571219062029076));
#29033=CARTESIAN_POINT('Ctrl Pts',(-0.218073051645397,-0.008746501642567,
-0.570903626238245));
#29034=CARTESIAN_POINT('Ctrl Pts',(-0.21370995744866,-0.089316201135509,
-0.567948038805485));
#29035=CARTESIAN_POINT('Ctrl Pts',(-0.113392555850513,-0.230857804862319,
-0.562352299730795));
#29036=CARTESIAN_POINT('Ctrl Pts',(0.131960746075832,-0.220770376824587,
-0.554431844805011));
#29037=CARTESIAN_POINT('Ctrl Pts',(0.25702911668245,-0.00944621435284863,
-0.546511389879224));
#29038=CARTESIAN_POINT('Ctrl Pts',(0.14781016650087,0.21048836658387,-0.538590934953439));
#29039=CARTESIAN_POINT('Ctrl Pts',(-0.096140787360785,0.238558476675654,
-0.530670480027653));
#29040=CARTESIAN_POINT('Ctrl Pts',(-0.210423490408626,0.100102627577536,
-0.524879855719531));
#29041=CARTESIAN_POINT('Ctrl Pts',(-0.217987512784609,0.0141353208686995,
-0.521729383053339));
#29042=CARTESIAN_POINT('Ctrl Pts',(-0.217860768206988,0.000187955723751776,
-0.521219062029076));
#29043=CARTESIAN_POINT('Origin',(0.,0.,-1.25608093797092));
#29044=CARTESIAN_POINT('',(-0.217759961965208,0.000196790833347493,-0.631080937970923));
#29045=CARTESIAN_POINT('',(-0.217447838183704,-7.77780874032519E-5,-0.621219062029076));
#29046=CARTESIAN_POINT('',(-0.217775,1.66341393608259E-15,-1.25608093797092));
#29047=CARTESIAN_POINT('Ctrl Pts',(-0.217759961965208,0.00019679083334749,
-0.631080937970923));
#29048=CARTESIAN_POINT('Ctrl Pts',(-0.217261836200481,-0.0547288371588338,
-0.629073646996136));
#29049=CARTESIAN_POINT('Ctrl Pts',(-0.168361205872163,-0.182687127116978,
-0.62442620437942));
#29050=CARTESIAN_POINT('Ctrl Pts',(0.046362713408588,-0.252989524617473,
-0.617138610120775));
#29051=CARTESIAN_POINT('Ctrl Pts',(0.237472868244547,-0.0987918903984044,
-0.609218155194989));
#29052=CARTESIAN_POINT('Ctrl Pts',(0.212121624547043,0.145456581701572,
-0.601297700269203));
#29053=CARTESIAN_POINT('Ctrl Pts',(-0.00658283818582227,0.257118391022893,
-0.593377245343417));
#29054=CARTESIAN_POINT('Ctrl Pts',(-0.187556770995067,0.152716308596067,
-0.586638324577325));
#29055=CARTESIAN_POINT('Ctrl Pts',(-0.217336457871426,0.0400011442544223,
-0.58253955545316));
#29056=CARTESIAN_POINT('Ctrl Pts',(-0.217437245756766,-6.08897400841621E-5,
-0.581080937970923));
#29057=CARTESIAN_POINT('Ctrl Pts',(-0.217447838183704,-7.77780874032311E-5,
-0.621219062029076));
#29058=CARTESIAN_POINT('Ctrl Pts',(-0.21754884652787,-0.0314176788091657,
-0.620077869423149));
#29059=CARTESIAN_POINT('Ctrl Pts',(-0.196570461683961,-0.135133614342587,
-0.616296525175294));
#29060=CARTESIAN_POINT('Ctrl Pts',(-0.0372308004467332,-0.254493743118089,
-0.609875029285512));
#29061=CARTESIAN_POINT('Ctrl Pts',(0.193239890732311,-0.169739631253061,
-0.601954574359726));
#29062=CARTESIAN_POINT('Ctrl Pts',(0.247568451193101,0.0697356419774633,
-0.594034119433939));
#29063=CARTESIAN_POINT('Ctrl Pts',(0.0762332818385088,0.245645444753797,
-0.586113664508155));
#29064=CARTESIAN_POINT('Ctrl Pts',(-0.154999187721833,0.199556042356295,
-0.578508645373198));
#29065=CARTESIAN_POINT('Ctrl Pts',(-0.217531913509314,0.063283441872864,
-0.573543777880173));
#29066=CARTESIAN_POINT('Ctrl Pts',(-0.218008398413668,-0.000140623921195505,
-0.571219062029076));
#29067=CARTESIAN_POINT('Origin',(0.,0.,-1.25608093797092));
#29068=CARTESIAN_POINT('',(-0.218079223833456,-9.27439839933367E-5,-0.681080937970923));
#29069=CARTESIAN_POINT('',(-0.217727166021048,0.000196079222951083,-0.671219062029076));
#29070=CARTESIAN_POINT('',(-0.217775,1.66341393608259E-15,-1.25608093797092));
#29071=CARTESIAN_POINT('Ctrl Pts',(-0.218079223833456,-9.27439839933141E-5,
-0.681080937970923));
#29072=CARTESIAN_POINT('Ctrl Pts',(-0.218107480872696,-0.00535093009861154,
-0.680888041822969));
#29073=CARTESIAN_POINT('Ctrl Pts',(-0.215555236352238,-0.0825495299588023,
-0.678054994033087));
#29074=CARTESIAN_POINT('Ctrl Pts',(-0.12393258111715,-0.225375056513412,
-0.672581794601276));
#29075=CARTESIAN_POINT('Ctrl Pts',(0.121624804919859,-0.226628788085249,
-0.664661339675491));
#29076=CARTESIAN_POINT('Ctrl Pts',(0.256318682363535,-0.0213057229917977,
-0.656740884749704));
#29077=CARTESIAN_POINT('Ctrl Pts',(0.157372814497323,0.203437946357048,
-0.648820429823919));
#29078=CARTESIAN_POINT('Ctrl Pts',(-0.0850216071723404,0.242743747755972,
-0.640899974898132));
#29079=CARTESIAN_POINT('Ctrl Pts',(-0.208127415665775,0.106898018501751,
-0.634986810947134));
#29080=CARTESIAN_POINT('Ctrl Pts',(-0.217917011544838,0.0175137966939258,
-0.631713798638064));
#29081=CARTESIAN_POINT('Ctrl Pts',(-0.217759961965208,0.00019679083334749,
-0.631080937970923));
#29082=CARTESIAN_POINT('Ctrl Pts',(-0.217727166021048,0.000196079222951085,
-0.671219062029076));
#29083=CARTESIAN_POINT('Ctrl Pts',(-0.217247214451338,-0.0536463720467488,
-0.669252112608055));
#29084=CARTESIAN_POINT('Ctrl Pts',(-0.169937424913778,-0.180512789837971,
-0.664645011545105));
#29085=CARTESIAN_POINT('Ctrl Pts',(0.0425099313519794,-0.253665337649058,
-0.657397758840227));
#29086=CARTESIAN_POINT('Ctrl Pts',(0.235942990845232,-0.102391908172312,
-0.64947730391444));
#29087=CARTESIAN_POINT('Ctrl Pts',(0.21430916648743,0.142213849352388,-0.641556848988655));
#29088=CARTESIAN_POINT('Ctrl Pts',(-0.00267186632973278,0.257188761260045,
-0.633636394062868));
#29089=CARTESIAN_POINT('Ctrl Pts',(-0.18630534750758,0.154942534370808,
-0.62685713174301));
#29090=CARTESIAN_POINT('Ctrl Pts',(-0.217315163498106,0.0410872514881082,
-0.622718021065078));
#29091=CARTESIAN_POINT('Ctrl Pts',(-0.217447838183704,-7.77780874032311E-5,
-0.621219062029076));
#29092=CARTESIAN_POINT('Origin',(0.,0.,-1.25608093797092));
#29093=CARTESIAN_POINT('',(-0.217495430256374,-0.000124623133544632,-0.731080937970923));
#29094=CARTESIAN_POINT('',(-0.218096740120519,-7.46359541664299E-5,-0.721219062029076));
#29095=CARTESIAN_POINT('',(-0.217775,1.66341393608259E-15,-1.25608093797092));
#29096=CARTESIAN_POINT('Ctrl Pts',(-0.217495430256374,-0.000124623133544624,
-0.731080937970923));
#29097=CARTESIAN_POINT('Ctrl Pts',(-0.217641789012947,-0.0280839662935587,
-0.730062285007874));
#29098=CARTESIAN_POINT('Ctrl Pts',(-0.199669006852885,-0.128327541509715,
-0.726403480402897));
#29099=CARTESIAN_POINT('Ctrl Pts',(-0.0489435840216807,-0.252502923436333,
-0.720104524155992));
#29100=CARTESIAN_POINT('Ctrl Pts',(0.18519517074638,-0.178482350648465,
-0.712184069230205));
#29101=CARTESIAN_POINT('Ctrl Pts',(0.250524722350552,0.0582285518621306,
-0.70426361430442));
#29102=CARTESIAN_POINT('Ctrl Pts',(0.0874958422396386,0.241862932983866,
-0.696343159378634));
#29103=CARTESIAN_POINT('Ctrl Pts',(-0.149374512656238,0.205931212802491,
-0.688615600600802));
#29104=CARTESIAN_POINT('Ctrl Pts',(-0.217720729403906,0.0666173743561128,
-0.683528193464898));
#29105=CARTESIAN_POINT('Ctrl Pts',(-0.218079223833456,-9.27439839933141E-5,
-0.681080937970923));
#29106=CARTESIAN_POINT('Ctrl Pts',(-0.218096740120519,-7.46359541664186E-5,
-0.721219062029076));
#29107=CARTESIAN_POINT('Ctrl Pts',(-0.218115278524842,-0.0042322574475895,
-0.721066507434889));
#29108=CARTESIAN_POINT('Ctrl Pts',(-0.216126462641042,-0.0803247351229268,
-0.718273801198772));
#29109=CARTESIAN_POINT('Ctrl Pts',(-0.127345709562336,-0.223464243323681,
-0.712840943320728));
#29110=CARTESIAN_POINT('Ctrl Pts',(0.118164206801822,-0.228452222617896,
-0.704920488394942));
#29111=CARTESIAN_POINT('Ctrl Pts',(0.255965020858851,-0.0252013072059438,
-0.697000033469156));
#29112=CARTESIAN_POINT('Ctrl Pts',(0.160448459333854,0.201021117511452,
-0.68907957854337));
#29113=CARTESIAN_POINT('Ctrl Pts',(-0.0813201694554329,0.244008663427961,
-0.681159123617584));
#29114=CARTESIAN_POINT('Ctrl Pts',(-0.20733152168619,0.109136913690184,
-0.67520561811282));
#29115=CARTESIAN_POINT('Ctrl Pts',(-0.217891432808594,0.0186240354207517,
-0.671892264249983));
#29116=CARTESIAN_POINT('Ctrl Pts',(-0.217727166021048,0.000196079222951085,
-0.671219062029076));
#29117=CARTESIAN_POINT('Origin',(0.,0.,-1.25608093797092));
#29118=CARTESIAN_POINT('',(-0.217632492219457,0.000183354111511343,-0.781080937970924));
#29119=CARTESIAN_POINT('',(-0.21751582202118,-0.000138136452134785,-0.771219062029076));
#29120=CARTESIAN_POINT('',(-0.217775,1.66341393608259E-15,-1.25608093797092));
#29121=CARTESIAN_POINT('Ctrl Pts',(-0.217632492219457,0.000183354111511339,
-0.781080937970924));
#29122=CARTESIAN_POINT('Ctrl Pts',(-0.217225850738349,-0.0503605582290492,
-0.77923652819278));
#29123=CARTESIAN_POINT('Ctrl Pts',(-0.174560998031809,-0.173873973729166,
-0.774751966772707));
#29124=CARTESIAN_POINT('Ctrl Pts',(0.0307503329195962,-0.255357823036844,
-0.767627253710707));
#29125=CARTESIAN_POINT('Ctrl Pts',(0.230962826542383,-0.113178502889618,
-0.759706798784921));
#29126=CARTESIAN_POINT('Ctrl Pts',(0.220647958398849,0.132165348012261,
-0.751786343859134));
#29127=CARTESIAN_POINT('Ctrl Pts',(0.00920794273158324,0.257037768725599,
-0.743865888933349));
#29128=CARTESIAN_POINT('Ctrl Pts',(-0.182352457983248,0.161687891688101,
-0.736964086970612));
#29129=CARTESIAN_POINT('Ctrl Pts',(-0.217262455397384,0.0443812484840306,
-0.732702436649803));
#29130=CARTESIAN_POINT('Ctrl Pts',(-0.217495430256374,-0.000124623133544624,
-0.731080937970923));
#29131=CARTESIAN_POINT('Ctrl Pts',(-0.21751582202118,-0.000138136452134743,
-0.771219062029076));
#29132=CARTESIAN_POINT('Ctrl Pts',(-0.217672533053156,-0.0269838912366882,
-0.770240750619793));
#29133=CARTESIAN_POINT('Ctrl Pts',(-0.200644381604158,-0.126086035057239,
-0.766622287568582));
#29134=CARTESIAN_POINT('Ctrl Pts',(-0.0527779420396886,-0.251729391653449,
-0.760363672875443));
#29135=CARTESIAN_POINT('Ctrl Pts',(0.182459421962995,-0.181278120922218,
-0.752443217949657));
#29136=CARTESIAN_POINT('Ctrl Pts',(0.251381274026667,0.0544118815782901,
-0.744522763023871));
#29137=CARTESIAN_POINT('Ctrl Pts',(0.0911639299237252,0.240504336071146,
-0.736602308098085));
#29138=CARTESIAN_POINT('Ctrl Pts',(-0.147464756036621,0.208010300530612,
-0.728834407766487));
#29139=CARTESIAN_POINT('Ctrl Pts',(-0.217794447815865,0.0677206802586771,
-0.723706659076817));
#29140=CARTESIAN_POINT('Ctrl Pts',(-0.218096740120519,-7.46359541664186E-5,
-0.721219062029076));
#29141=CARTESIAN_POINT('Origin',(0.,0.,-1.25608093797092));
#29142=CARTESIAN_POINT('',(-0.218127064665478,-1.51157432300434E-5,-0.831080937970924));
#29143=CARTESIAN_POINT('',(-0.217603720989924,0.0001758774262937,-0.821219062029076));
#29144=CARTESIAN_POINT('',(-0.217775,1.66341393608259E-15,-1.25608093797092));
#29145=CARTESIAN_POINT('Ctrl Pts',(-0.218127064665478,-1.51157432300175E-5,
-0.831080937970924));
#29146=CARTESIAN_POINT('Ctrl Pts',(-0.218127886525049,-0.000832818950451307,
-0.831050923019614));
#29147=CARTESIAN_POINT('Ctrl Pts',(-0.217754036594478,-0.0735759187401932,
-0.828380756426375));
#29148=CARTESIAN_POINT('Ctrl Pts',(-0.137529414910091,-0.217345027077388,
-0.823070438191206));
#29149=CARTESIAN_POINT('Ctrl Pts',(0.107488237249403,-0.233665315384629,
-0.815149983265423));
#29150=CARTESIAN_POINT('Ctrl Pts',(0.254528152697761,-0.0369948678203813,
-0.807229528339635));
#29151=CARTESIAN_POINT('Ctrl Pts',(0.169560427414887,0.193397161860414,
-0.79930907341385));
#29152=CARTESIAN_POINT('Ctrl Pts',(-0.0699651112530573,0.247503704958389,
-0.791388618488063));
#29153=CARTESIAN_POINT('Ctrl Pts',(-0.204789490261868,0.115941739323129,
-0.785312573340423));
#29154=CARTESIAN_POINT('Ctrl Pts',(-0.217807931351206,0.021989737641606,
-0.781876679834709));
#29155=CARTESIAN_POINT('Ctrl Pts',(-0.217632492219457,0.000183354111511339,
-0.781080937970924));
#29156=CARTESIAN_POINT('Ctrl Pts',(-0.217603720989924,0.000175877426293707,
-0.821219062029076));
#29157=CARTESIAN_POINT('Ctrl Pts',(-0.21722579264226,-0.0492790478079207,
-0.819414993804698));
#29158=CARTESIAN_POINT('Ctrl Pts',(-0.176029688244654,-0.171678173502806,
-0.814970773938393));
#29159=CARTESIAN_POINT('Ctrl Pts',(0.026863340058709,-0.25579593184617,
-0.807886402430158));
#29160=CARTESIAN_POINT('Ctrl Pts',(0.229214913121365,-0.116677853043863,
-0.799965947504372));
#29161=CARTESIAN_POINT('Ctrl Pts',(0.222632383413667,0.128794486076502,
-0.792045492578587));
#29162=CARTESIAN_POINT('Ctrl Pts',(0.0131158620091436,0.256868004920654,
-0.7841250376528));
#29163=CARTESIAN_POINT('Ctrl Pts',(-0.181000476366041,0.163902138278909,
-0.777182894136297));
#29164=CARTESIAN_POINT('Ctrl Pts',(-0.217249619771706,0.0454642708727976,
-0.772880902261722));
#29165=CARTESIAN_POINT('Ctrl Pts',(-0.21751582202118,-0.000138136452134743,
-0.771219062029076));
#29166=CARTESIAN_POINT('Origin',(0.,0.,-1.25608093797092));
#29167=CARTESIAN_POINT('',(-0.217590234620949,-0.000171676759354653,-0.881080937970924));
#29168=CARTESIAN_POINT('',(-0.21812823151327,5.20618463971455E-6,-0.871219062029076));
#29169=CARTESIAN_POINT('',(-0.217775,1.66341393608259E-15,-1.25608093797092));
#29170=CARTESIAN_POINT('Ctrl Pts',(-0.217590234620949,-0.000171676759354655,
-0.881080937970924));
#29171=CARTESIAN_POINT('Ctrl Pts',(-0.217764472112696,-0.0236346228518696,
-0.880225166204519));
#29172=CARTESIAN_POINT('Ctrl Pts',(-0.203474532729487,-0.119276866693917,
-0.876729242796186));
#29173=CARTESIAN_POINT('Ctrl Pts',(-0.0643464817567947,-0.249023555203761,
-0.870593167745921));
#29174=CARTESIAN_POINT('Ctrl Pts',(0.173893356378981,-0.189510689323927,
-0.862672712820138));
#29175=CARTESIAN_POINT('Ctrl Pts',(0.253625827354345,0.042745063570017,
-0.85475225789435));
#29176=CARTESIAN_POINT('Ctrl Pts',(0.102173145688224,0.236037812777863,
-0.846831802968565));
#29177=CARTESIAN_POINT('Ctrl Pts',(-0.141485588421475,0.214260087681797,
-0.838941362994089));
#29178=CARTESIAN_POINT('Ctrl Pts',(-0.218055594757132,0.0710933502062712,
-0.833691074661543));
#29179=CARTESIAN_POINT('Ctrl Pts',(-0.218127064665478,-1.51157432300175E-5,
-0.831080937970924));
#29180=CARTESIAN_POINT('Ctrl Pts',(-0.21812823151327,5.20618463970728E-6,
-0.871219062029076));
#29181=CARTESIAN_POINT('Ctrl Pts',(-0.218102942100602,-0.0716385923522861,
-0.868589236989604));
#29182=CARTESIAN_POINT('Ctrl Pts',(-0.140499760598608,-0.21525449840371,
-0.863319260308203));
#29183=CARTESIAN_POINT('Ctrl Pts',(0.103922264034112,-0.235272949626989,
-0.855409131984872));
#29184=CARTESIAN_POINT('Ctrl Pts',(0.25393610059609,-0.0408614072470928,
-0.847488677059087));
#29185=CARTESIAN_POINT('Ctrl Pts',(0.172481964081841,0.1907961473789,-0.839568222133301));
#29186=CARTESIAN_POINT('Ctrl Pts',(-0.0661930265154354,0.248539093562536,
-0.831647767207517));
#29187=CARTESIAN_POINT('Ctrl Pts',(-0.203910920659895,0.11818294676327,
-0.825531380506107));
#29188=CARTESIAN_POINT('Ctrl Pts',(-0.217778869368591,0.0230954335416578,
-0.822055145446627));
#29189=CARTESIAN_POINT('Ctrl Pts',(-0.217603720989924,0.000175877426293707,
-0.821219062029076));
#29190=CARTESIAN_POINT('Origin',(0.,0.,-1.25608093797092));
#29191=CARTESIAN_POINT('',(-0.217526565113027,0.000144321015786189,-0.931080937970924));
#29192=CARTESIAN_POINT('',(-0.217618267924705,-0.000179898412300761,-0.921219062029076));
#29193=CARTESIAN_POINT('',(-0.217775,1.66341393608259E-15,-1.25608093797092));
#29194=CARTESIAN_POINT('Ctrl Pts',(-0.217526565113027,0.000144321015786177,
-0.931080937970924));
#29195=CARTESIAN_POINT('Ctrl Pts',(-0.217244272156895,-0.0459926317880253,
-0.929399409389424));
#29196=CARTESIAN_POINT('Ctrl Pts',(-0.180331437388558,-0.164981497104693,
-0.925077729165994));
#29197=CARTESIAN_POINT('Ctrl Pts',(0.0150220433400717,-0.256763585765983,
-0.918115897300639));
#29198=CARTESIAN_POINT('Ctrl Pts',(0.22358220268487,-0.127138504801763,
-0.910195442374852));
#29199=CARTESIAN_POINT('Ctrl Pts',(0.228342590551659,0.118375935480206,
-0.902274987449066));
#29200=CARTESIAN_POINT('Ctrl Pts',(0.0249640155933997,0.255988278415915,
-0.894354532523281));
#29201=CARTESIAN_POINT('Ctrl Pts',(-0.176736969944704,0.170604861907604,
-0.887289849363898));
#29202=CARTESIAN_POINT('Ctrl Pts',(-0.217226929957205,0.0487511908457016,
-0.882865317846447));
#29203=CARTESIAN_POINT('Ctrl Pts',(-0.217590234620949,-0.000171676759354655,
-0.881080937970924));
#29204=CARTESIAN_POINT('Ctrl Pts',(-0.217618267924705,-0.000179898412300724,
-0.921219062029077));
#29205=CARTESIAN_POINT('Ctrl Pts',(-0.217793826238208,-0.0225295119375463,
-0.920403631816438));
#29206=CARTESIAN_POINT('Ctrl Pts',(-0.20436332104689,-0.117035495875518,
-0.916948049961871));
#29207=CARTESIAN_POINT('Ctrl Pts',(-0.0681261445426857,-0.248016181363272,
-0.910852316465374));
#29208=CARTESIAN_POINT('Ctrl Pts',(0.170991197855606,-0.192133308002639,
-0.902931861539589));
#29209=CARTESIAN_POINT('Ctrl Pts',(0.254246550215305,0.0388830231818767,
-0.895011406613802));
#29210=CARTESIAN_POINT('Ctrl Pts',(0.105750948292417,0.234456679843913,
-0.887090951688017));
#29211=CARTESIAN_POINT('Ctrl Pts',(-0.139138815762931,0.216318255670307,
-0.879170496762231));
#29212=CARTESIAN_POINT('Ctrl Pts',(-0.218000660033129,0.072492888641203,
-0.873879866875917));
#29213=CARTESIAN_POINT('Ctrl Pts',(-0.218128330817865,0.000286531753771226,
-0.871229388631533));
#29214=CARTESIAN_POINT('Ctrl Pts',(-0.21812823151327,5.20618463970728E-6,
-0.871219062029076));
#29215=CARTESIAN_POINT('Origin',(0.,0.,-1.25608093797092));
#29216=CARTESIAN_POINT('',(-0.218104054822873,6.54679023023512E-5,-0.981080937970924));
#29217=CARTESIAN_POINT('',(-0.2175051044321,0.000131354540280196,-0.971219062029076));
#29218=CARTESIAN_POINT('',(-0.217775,1.66341393608259E-15,-1.25608093797092));
#29219=CARTESIAN_POINT('Ctrl Pts',(-0.218104054822873,6.54679023023327E-5,
-0.981080937970924));
#29220=CARTESIAN_POINT('Ctrl Pts',(-0.217832592967684,-0.0682603177041455,
-0.978573652574329));
#29221=CARTESIAN_POINT('Ctrl Pts',(-0.146522207495947,-0.209021230560728,
-0.973426215535804));
#29222=CARTESIAN_POINT('Ctrl Pts',(0.092946507651719,-0.239821073941797,
-0.965638626855354));
#29223=CARTESIAN_POINT('Ctrl Pts',(0.251778214672948,-0.05254456561971,
-0.957718171929568));
#29224=CARTESIAN_POINT('Ctrl Pts',(0.181108905951714,0.182627393722108,
-0.949797717003781));
#29225=CARTESIAN_POINT('Ctrl Pts',(-0.0546448916053246,0.251330731481492,
-0.941877262077996));
#29226=CARTESIAN_POINT('Ctrl Pts',(-0.201112491437176,0.124992019589862,
-0.93563833573371));
#29227=CARTESIAN_POINT('Ctrl Pts',(-0.217687497576811,0.026446548276287,
-0.932039561031353));
#29228=CARTESIAN_POINT('Ctrl Pts',(-0.217526565113027,0.000144321015786177,
-0.931080937970924));
#29229=CARTESIAN_POINT('Ctrl Pts',(-0.2175051044321,0.000131354540280217,
-0.971219062029076));
#29230=CARTESIAN_POINT('Ctrl Pts',(-0.217255883023214,-0.0449098808917798,
-0.969577875001342));
#29231=CARTESIAN_POINT('Ctrl Pts',(-0.18169579707604,-0.162768967076207,
-0.96529653633168));
#29232=CARTESIAN_POINT('Ctrl Pts',(0.0111154911491714,-0.256962338971068,
-0.958375046020089));
#29233=CARTESIAN_POINT('Ctrl Pts',(0.221622841759585,-0.130523997019855,
-0.950454591094304));
#29234=CARTESIAN_POINT('Ctrl Pts',(0.230116418626786,0.114889649949471,
-0.942534136168517));
#29235=CARTESIAN_POINT('Ctrl Pts',(0.0288541519363172,0.255579020471033,
-0.934613681242733));
#29236=CARTESIAN_POINT('Ctrl Pts',(-0.175281056344178,0.172802918894569,
-0.927508656529584));
#29237=CARTESIAN_POINT('Ctrl Pts',(-0.21722541392963,0.0498327428950334,
-0.923043783458366));
#29238=CARTESIAN_POINT('Ctrl Pts',(-0.217618267924705,-0.000179898412300724,
-0.921219062029077));
#29239=CARTESIAN_POINT('Origin',(0.,0.,-1.25608093797092));
#29240=CARTESIAN_POINT('',(-0.217711384278981,-0.000195092093718535,-1.03108093797092));
#29241=CARTESIAN_POINT('',(-0.218088181886173,8.40274599361677E-5,-1.02121906202908));
#29242=CARTESIAN_POINT('',(-0.217775,1.66341393608259E-15,-1.25608093797092));
#29243=CARTESIAN_POINT('Ctrl Pts',(-0.217711384278981,-0.000195092093718539,
-1.03108093797092));
#29244=CARTESIAN_POINT('Ctrl Pts',(-0.217878581251591,-0.0191654947610302,
-1.03038804740116));
#29245=CARTESIAN_POINT('Ctrl Pts',(-0.206935794297685,-0.110229868580331,
-1.02705500518947));
#29246=CARTESIAN_POINT('Ctrl Pts',(-0.0795068333803697,-0.244605521341649,
-1.02108181133586));
#29247=CARTESIAN_POINT('Ctrl Pts',(0.161936074723358,-0.199824697090791,
-1.01316135641007));
#29248=CARTESIAN_POINT('Ctrl Pts',(0.25577092546644,0.0271004554068604,
-1.00524090148428));
#29249=CARTESIAN_POINT('Ctrl Pts',(0.116465321567834,0.229322980077886,
-0.997320446558497));
#29250=CARTESIAN_POINT('Ctrl Pts',(-0.129000815316647,0.222512899840908,
-0.98939999163271));
#29251=CARTESIAN_POINT('Ctrl Pts',(-0.216398828568288,0.0792394791905274,
-0.98398682210352));
#29252=CARTESIAN_POINT('Ctrl Pts',(-0.218118440148731,0.00368619277284598,
-0.981213804216257));
#29253=CARTESIAN_POINT('Ctrl Pts',(-0.218104054822873,6.54679023023327E-5,
-0.981080937970924));
#29254=CARTESIAN_POINT('Ctrl Pts',(-0.218088181886173,8.40274599361686E-5,
-1.02121906202908));
#29255=CARTESIAN_POINT('Ctrl Pts',(-0.217755967501094,-0.0671554398934883,
-1.01875211818625));
#29256=CARTESIAN_POINT('Ctrl Pts',(-0.148446081963974,-0.206947166699799,
-1.01364502270149));
#29257=CARTESIAN_POINT('Ctrl Pts',(0.0892886006322762,-0.241206848519812,
-1.0058977755748));
#29258=CARTESIAN_POINT('Ctrl Pts',(0.250950003708668,-0.0563674856785394,
-0.997977320649019));
#29259=CARTESIAN_POINT('Ctrl Pts',(0.183865322083874,0.179851997660945,
-0.990056865723231));
#29260=CARTESIAN_POINT('Ctrl Pts',(-0.0508163781729916,0.252132690320144,
-0.982136410797448));
#29261=CARTESIAN_POINT('Ctrl Pts',(-0.200147761824428,0.127233622778126,
-0.975857142899395));
#29262=CARTESIAN_POINT('Ctrl Pts',(-0.217656801566168,0.0275472429283243,
-0.972218026643271));
#29263=CARTESIAN_POINT('Ctrl Pts',(-0.2175051044321,0.000131354540280217,
-0.971219062029076));
#29264=CARTESIAN_POINT('Origin',(0.,0.,-1.25608093797092));
#29265=CARTESIAN_POINT('',(-0.217453911095485,8.60469890504272E-5,-1.08108093797092));
#29266=CARTESIAN_POINT('',(-0.217743889400727,-0.000196664163112259,-1.07121906202908));
#29267=CARTESIAN_POINT('',(-0.217775,1.66341393608259E-15,-1.25608093797092));
#29268=CARTESIAN_POINT('Ctrl Pts',(-0.217453911095485,8.60469890503895E-5,
-1.08108093797092));
#29269=CARTESIAN_POINT('Ctrl Pts',(-0.217305410614029,-0.0416168581794606,
-1.07956229058607));
#29270=CARTESIAN_POINT('Ctrl Pts',(-0.185685765260903,-0.156028526245301,
-1.07540349155928));
#29271=CARTESIAN_POINT('Ctrl Pts',(-0.000762821507371324,-0.25720122800503,
-1.06860454089057));
#29272=CARTESIAN_POINT('Ctrl Pts',(0.215358791521507,-0.140619426360152,
-1.06068408596478));
#29273=CARTESIAN_POINT('Ctrl Pts',(0.235176530521566,0.104140400581766,
-1.052763631039));
#29274=CARTESIAN_POINT('Ctrl Pts',(0.0406259830504325,0.253973834313976,
-1.04484317611321));
#29275=CARTESIAN_POINT('Ctrl Pts',(-0.17069690156357,0.1794495265795,-1.03761561175719));
#29276=CARTESIAN_POINT('Ctrl Pts',(-0.217241503217881,0.0531182711551457,
-1.03302819904309));
#29277=CARTESIAN_POINT('Ctrl Pts',(-0.217711384278981,-0.000195092093718539,
-1.03108093797092));
#29278=CARTESIAN_POINT('Ctrl Pts',(-0.217743889400727,-0.000196664163112275,
-1.07121906202908));
#29279=CARTESIAN_POINT('Ctrl Pts',(-0.217904661477969,-0.0180557774320445,
-1.07056651301308));
#29280=CARTESIAN_POINT('Ctrl Pts',(-0.207741505551685,-0.107990640708861,
-1.06727381235516));
#29281=CARTESIAN_POINT('Ctrl Pts',(-0.0832175410220989,-0.243368068736343,
-1.06134096005531));
#29282=CARTESIAN_POINT('Ctrl Pts',(0.158878438899101,-0.202264296402348,
-1.05342050512952));
#29283=CARTESIAN_POINT('Ctrl Pts',(0.25615348338552,0.0232076117179531,
-1.04550005020373));
#29284=CARTESIAN_POINT('Ctrl Pts',(0.119939351168713,0.227525266045112,
-1.03757959527795));
#29285=CARTESIAN_POINT('Ctrl Pts',(-0.125601956730251,0.224448986095295,
-1.02965914035216));
#29286=CARTESIAN_POINT('Ctrl Pts',(-0.215836233287728,0.081463554320085,
-1.0242056292692));
#29287=CARTESIAN_POINT('Ctrl Pts',(-0.21811150715263,0.00480501054465392,
-1.02139226982818));
#29288=CARTESIAN_POINT('Ctrl Pts',(-0.218088181886173,8.40274599361686E-5,
-1.02121906202908));
#29289=CARTESIAN_POINT('Origin',(0.,0.,-1.25608093797092));
#29290=CARTESIAN_POINT('',(-0.21801873929181,0.00014895038204359,-1.13108093797092));
#29291=CARTESIAN_POINT('',(-0.217441534898734,7.07751596318168E-5,-1.12121906202908));
#29292=CARTESIAN_POINT('',(-0.217775,1.66341393608259E-15,-1.25608093797092));
#29293=CARTESIAN_POINT('Ctrl Pts',(-0.21801873929181,0.000148950382043584,
-1.13108093797092));
#29294=CARTESIAN_POINT('Ctrl Pts',(-0.217555670191414,-0.0637989277634247,
-1.12873653377097));
#29295=CARTESIAN_POINT('Ctrl Pts',(-0.154117328807783,-0.200610241566758,
-1.12375197792909));
#29296=CARTESIAN_POINT('Ctrl Pts',(0.0780566987792774,-0.245059402025012,
-1.11612727044528));
#29297=CARTESIAN_POINT('Ctrl Pts',(0.248078039310978,-0.0679032867325597,
-1.1082068155195));
#29298=CARTESIAN_POINT('Ctrl Pts',(0.191975348375761,0.171172964635631,
-1.10028636059371));
#29299=CARTESIAN_POINT('Ctrl Pts',(-0.0391190265108933,0.254208440109437,
-1.09236590566793));
#29300=CARTESIAN_POINT('Ctrl Pts',(-0.197082164878129,0.134040930345383,
-1.085964098127));
#29301=CARTESIAN_POINT('Ctrl Pts',(-0.217563577054673,0.0308831801123549,
-1.082202442228));
#29302=CARTESIAN_POINT('Ctrl Pts',(-0.217453911095485,8.60469890503895E-5,
-1.08108093797092));
#29303=CARTESIAN_POINT('Ctrl Pts',(-0.217441534898734,7.07751596318099E-5,
-1.12121906202908));
#29304=CARTESIAN_POINT('Ctrl Pts',(-0.217325562139716,-0.0405305200113168,
-1.11974075619799));
#29305=CARTESIAN_POINT('Ctrl Pts',(-0.186950053002431,-0.153805877485014,
-1.11562229872497));
#29306=CARTESIAN_POINT('Ctrl Pts',(-0.00467359635069057,-0.257158283796502,
-1.10886368961002));
#29307=CARTESIAN_POINT('Ctrl Pts',(0.213195046788718,-0.143879137770345,
-1.10094323468424));
#29308=CARTESIAN_POINT('Ctrl Pts',(0.236733244856063,0.100552273737884,
-1.09302277975845));
#29309=CARTESIAN_POINT('Ctrl Pts',(0.0444835839728878,0.253326392640624,
-1.08510232483266));
#29310=CARTESIAN_POINT('Ctrl Pts',(-0.169133800272843,0.181626810356099,
-1.07783441892287));
#29311=CARTESIAN_POINT('Ctrl Pts',(-0.217254192849094,0.054200506869408,
-1.07320666465501));
#29312=CARTESIAN_POINT('Ctrl Pts',(-0.217743889400727,-0.000196664163112275,
-1.07121906202908));
#29313=CARTESIAN_POINT('Origin',(0.03,0.28,0.6));
#29314=CARTESIAN_POINT('',(0.03,0.28,0.6));
#29315=CARTESIAN_POINT('',(-0.03,0.28,0.6));
#29316=CARTESIAN_POINT('',(0.015,0.28,0.6));
#29317=CARTESIAN_POINT('',(0.03,0.28,0.57));
#29318=CARTESIAN_POINT('',(0.03,0.28,0.6));
#29319=CARTESIAN_POINT('',(-0.03,0.28,0.57));
#29320=CARTESIAN_POINT('',(-0.03,0.28,0.57));
#29321=CARTESIAN_POINT('',(-0.03,0.28,0.6));
#29322=CARTESIAN_POINT('Origin',(0.03,0.42,0.6));
#29323=CARTESIAN_POINT('',(0.03,0.42,0.6));
#29324=CARTESIAN_POINT('',(0.03,0.21,0.6));
#29325=CARTESIAN_POINT('',(0.03,0.42,0.57));
#29326=CARTESIAN_POINT('',(0.03,0.42,0.6));
#29327=CARTESIAN_POINT('',(0.03,0.28,0.57));
#29328=CARTESIAN_POINT('Origin',(-0.03,0.42,0.6));
#29329=CARTESIAN_POINT('',(-0.03,0.42,0.6));
#29330=CARTESIAN_POINT('',(-0.015,0.42,0.6));
#29331=CARTESIAN_POINT('',(-0.03,0.42,0.57));
#29332=CARTESIAN_POINT('',(-0.03,0.42,0.6));
#29333=CARTESIAN_POINT('',(0.03,0.42,0.57));
#29334=CARTESIAN_POINT('Origin',(-0.03,0.28,0.6));
#29335=CARTESIAN_POINT('',(-0.03,0.14,0.6));
#29336=CARTESIAN_POINT('',(-0.03,0.42,0.57));
#29337=CARTESIAN_POINT('Origin',(0.,0.35,0.57));
#29338=CARTESIAN_POINT('Origin',(0.,0.,-1.2));
#29339=CARTESIAN_POINT('',(-0.151,-1.8492166667125E-17,-1.2));
#29340=CARTESIAN_POINT('Origin',(0.,0.,-1.2));
#29341=CARTESIAN_POINT('',(-0.151,-1.8492166667125E-17,-1.05));
#29342=CARTESIAN_POINT('',(-0.151,-1.8492166667125E-17,-1.2));
#29343=CARTESIAN_POINT('Origin',(0.,0.,-1.05));
#29344=CARTESIAN_POINT('Origin',(0.,0.,-1.05));
#29345=CARTESIAN_POINT('Ctrl Pts',(-0.0944853208817847,0.196210282000883,
-1.18014778394209));
#29346=CARTESIAN_POINT('Ctrl Pts',(-0.159582249462734,0.164862769920135,
-1.17750763230016));
#29347=CARTESIAN_POINT('Ctrl Pts',(-0.255023143260422,0.0328527272961977,
-1.17222732901631));
#29348=CARTESIAN_POINT('Ctrl Pts',(-0.166183579550698,-0.196528621075993,
-1.16430687409052));
#29349=CARTESIAN_POINT('Ctrl Pts',(0.0743494844831576,-0.246142736672221,
-1.15638641916474));
#29350=CARTESIAN_POINT('Ctrl Pts',(0.247001644414856,-0.0717076563344237,
-1.14846596423895));
#29351=CARTESIAN_POINT('Ctrl Pts',(0.194564222666998,0.168254406153596,
-1.14054550931316));
#29352=CARTESIAN_POINT('Ctrl Pts',(-0.0352527091661894,0.254763023235567,
-1.13262505438738));
#29353=CARTESIAN_POINT('Ctrl Pts',(-0.232920168884155,0.109095201333321,
-1.12470459946159));
#29354=CARTESIAN_POINT('Ctrl Pts',(-0.218284479061633,-0.136038973337895,
-1.11678414453581));
#29355=CARTESIAN_POINT('Ctrl Pts',(-0.00467359635069057,-0.257158283796502,
-1.10886368961002));
#29356=CARTESIAN_POINT('Ctrl Pts',(0.213195046788718,-0.143879137770345,
-1.10094323468424));
#29357=CARTESIAN_POINT('Ctrl Pts',(0.236733244856063,0.100552273737884,
-1.09302277975845));
#29358=CARTESIAN_POINT('Ctrl Pts',(0.0444835839728878,0.253326392640624,
-1.08510232483266));
#29359=CARTESIAN_POINT('Ctrl Pts',(-0.188313439582864,0.175189262533144,
-1.07718186990688));
#29360=CARTESIAN_POINT('Ctrl Pts',(-0.249459071805079,-0.0626369865404807,
-1.06926141498109));
#29361=CARTESIAN_POINT('Ctrl Pts',(-0.0832175410220989,-0.243368068736343,
-1.06134096005531));
#29362=CARTESIAN_POINT('Ctrl Pts',(0.158878438899101,-0.202264296402348,
-1.05342050512952));
#29363=CARTESIAN_POINT('Ctrl Pts',(0.25615348338552,0.0232076117179531,
-1.04550005020373));
#29364=CARTESIAN_POINT('Ctrl Pts',(0.119939351168713,0.227525266045112,
-1.03757959527795));
#29365=CARTESIAN_POINT('Ctrl Pts',(-0.125601956730251,0.224448986095295,
-1.02965914035216));
#29366=CARTESIAN_POINT('Ctrl Pts',(-0.256654504229033,0.0167828330074643,
-1.02173868542638));
#29367=CARTESIAN_POINT('Ctrl Pts',(-0.15376119589656,-0.206181211517413,
-1.01381823050059));
#29368=CARTESIAN_POINT('Ctrl Pts',(0.0892886006322762,-0.241206848519812,
-1.0058977755748));
#29369=CARTESIAN_POINT('Ctrl Pts',(0.250950003708668,-0.0563674856785394,
-0.997977320649019));
#29370=CARTESIAN_POINT('Ctrl Pts',(0.183865322083874,0.179851997660945,
-0.990056865723231));
#29371=CARTESIAN_POINT('Ctrl Pts',(-0.0508163781729916,0.252132690320144,
-0.982136410797448));
#29372=CARTESIAN_POINT('Ctrl Pts',(-0.239177905729943,0.0945892551935581,
-0.974215955871661));
#29373=CARTESIAN_POINT('Ctrl Pts',(-0.209523858011382,-0.14917422935663,
-0.966295500945875));
#29374=CARTESIAN_POINT('Ctrl Pts',(0.0111154911491714,-0.256962338971068,
-0.958375046020089));
#29375=CARTESIAN_POINT('Ctrl Pts',(0.221622841759585,-0.130523997019855,
-0.950454591094304));
#29376=CARTESIAN_POINT('Ctrl Pts',(0.230116418626786,0.114889649949471,
-0.942534136168517));
#29377=CARTESIAN_POINT('Ctrl Pts',(0.0288541519363172,0.255579020471033,
-0.934613681242733));
#29378=CARTESIAN_POINT('Ctrl Pts',(-0.198709267084557,0.163302862689978,
-0.926693226316945));
#29379=CARTESIAN_POINT('Ctrl Pts',(-0.245145106467147,-0.0778272096586138,
-0.918772771391161));
#29380=CARTESIAN_POINT('Ctrl Pts',(-0.0681261445426857,-0.248016181363272,
-0.910852316465374));
#29381=CARTESIAN_POINT('Ctrl Pts',(0.170991197855606,-0.192133308002639,
-0.902931861539589));
#29382=CARTESIAN_POINT('Ctrl Pts',(0.254246550215305,0.0388830231818767,
-0.895011406613802));
#29383=CARTESIAN_POINT('Ctrl Pts',(0.105750948292417,0.234456679843913,
-0.887090951688017));
#29384=CARTESIAN_POINT('Ctrl Pts',(-0.139138815762931,0.216318255670307,
-0.879170496762231));
#29385=CARTESIAN_POINT('Ctrl Pts',(-0.25720069049779,0.00100129696836331,
-0.871250041836445));
#29386=CARTESIAN_POINT('Ctrl Pts',(-0.140818851386615,-0.215228364492966,
-0.86332958691066));
#29387=CARTESIAN_POINT('Ctrl Pts',(0.103922264034112,-0.235272949626989,
-0.855409131984872));
#29388=CARTESIAN_POINT('Ctrl Pts',(0.25393610059609,-0.0408614072470928,
-0.847488677059087));
#29389=CARTESIAN_POINT('Ctrl Pts',(0.172481964081841,0.1907961473789,-0.839568222133301));
#29390=CARTESIAN_POINT('Ctrl Pts',(-0.0661930265154354,0.248539093562536,
-0.831647767207517));
#29391=CARTESIAN_POINT('Ctrl Pts',(-0.244531713438901,0.0797335494681849,
-0.823727312281729));
#29392=CARTESIAN_POINT('Ctrl Pts',(-0.19997471940289,-0.161750763175621,
-0.815806857355944));
#29393=CARTESIAN_POINT('Ctrl Pts',(0.026863340058709,-0.25579593184617,
-0.807886402430158));
#29394=CARTESIAN_POINT('Ctrl Pts',(0.229214913121365,-0.116677853043863,
-0.799965947504372));
#29395=CARTESIAN_POINT('Ctrl Pts',(0.222632383413667,0.128794486076502,
-0.792045492578587));
#29396=CARTESIAN_POINT('Ctrl Pts',(0.0131158620091436,0.256868004920654,
-0.7841250376528));
#29397=CARTESIAN_POINT('Ctrl Pts',(-0.208356037095823,0.150801059657697,
-0.776204582727015));
#29398=CARTESIAN_POINT('Ctrl Pts',(-0.239907127495152,-0.0927241498488127,
-0.768284127801228));
#29399=CARTESIAN_POINT('Ctrl Pts',(-0.0527779420396886,-0.251729391653449,
-0.760363672875443));
#29400=CARTESIAN_POINT('Ctrl Pts',(0.182459421962995,-0.181278120922218,
-0.752443217949657));
#29401=CARTESIAN_POINT('Ctrl Pts',(0.251381274026667,0.0544118815782901,
-0.744522763023871));
#29402=CARTESIAN_POINT('Ctrl Pts',(0.0911639299237252,0.240504336071146,
-0.736602308098085));
#29403=CARTESIAN_POINT('Ctrl Pts',(-0.152151209363023,0.207372146821915,
-0.7286818531723));
#29404=CARTESIAN_POINT('Ctrl Pts',(-0.256777395209575,-0.0147840149332312,
-0.720761398246514));
#29405=CARTESIAN_POINT('Ctrl Pts',(-0.127345709562336,-0.223464243323681,
-0.712840943320728));
#29406=CARTESIAN_POINT('Ctrl Pts',(0.118164206801822,-0.228452222617896,
-0.704920488394942));
#29407=CARTESIAN_POINT('Ctrl Pts',(0.255965020858851,-0.0252013072059438,
-0.697000033469156));
#29408=CARTESIAN_POINT('Ctrl Pts',(0.160448459333854,0.201021117511452,
-0.68907957854337));
#29409=CARTESIAN_POINT('Ctrl Pts',(-0.0813201694554329,0.244008663427961,
-0.681159123617584));
#29410=CARTESIAN_POINT('Ctrl Pts',(-0.248963792978122,0.0645772992165747,
-0.673238668691798));
#29411=CARTESIAN_POINT('Ctrl Pts',(-0.189671803979623,-0.173717600038902,
-0.665318213766012));
#29412=CARTESIAN_POINT('Ctrl Pts',(0.0425099313519794,-0.253665337649058,
-0.657397758840227));
#29413=CARTESIAN_POINT('Ctrl Pts',(0.235942990845232,-0.102391908172312,
-0.64947730391444));
#29414=CARTESIAN_POINT('Ctrl Pts',(0.21430916648743,0.142213849352388,-0.641556848988655));
#29415=CARTESIAN_POINT('Ctrl Pts',(-0.00267186632973278,0.257188761260045,
-0.633636394062868));
#29416=CARTESIAN_POINT('Ctrl Pts',(-0.217217438091055,0.137730833066962,
-0.625715939137084));
#29417=CARTESIAN_POINT('Ctrl Pts',(-0.233764852072829,-0.107271579290737,
-0.617795484211297));
#29418=CARTESIAN_POINT('Ctrl Pts',(-0.0372308004467332,-0.254493743118089,
-0.609875029285512));
#29419=CARTESIAN_POINT('Ctrl Pts',(0.193239890732311,-0.169739631253061,
-0.601954574359726));
#29420=CARTESIAN_POINT('Ctrl Pts',(0.247568451193101,0.0697356419774633,
-0.594034119433939));
#29421=CARTESIAN_POINT('Ctrl Pts',(0.0762332818385088,0.245645444753797,
-0.586113664508155));
#29422=CARTESIAN_POINT('Ctrl Pts',(-0.164590090204428,0.197644377594352,
-0.578193209582367));
#29423=CARTESIAN_POINT('Ctrl Pts',(-0.255386213350406,-0.0305136005528887,
-0.570272754656583));
#29424=CARTESIAN_POINT('Ctrl Pts',(-0.113392555850513,-0.230857804862319,
-0.562352299730795));
#29425=CARTESIAN_POINT('Ctrl Pts',(0.131960746075832,-0.220770376824587,
-0.554431844805011));
#29426=CARTESIAN_POINT('Ctrl Pts',(0.25702911668245,-0.00944621435284863,
-0.546511389879224));
#29427=CARTESIAN_POINT('Ctrl Pts',(0.14781016650087,0.21048836658387,-0.538590934953439));
#29428=CARTESIAN_POINT('Ctrl Pts',(-0.096140787360785,0.238558476675654,
-0.530670480027653));
#29429=CARTESIAN_POINT('Ctrl Pts',(-0.25245743823001,0.0491776338440616,
-0.522750025101866));
#29430=CARTESIAN_POINT('Ctrl Pts',(-0.178653947150355,-0.185029632642338,
-0.514829570176082));
#29431=CARTESIAN_POINT('Ctrl Pts',(0.0579962873891273,-0.250578587347838,
-0.506909115250295));
#29432=CARTESIAN_POINT('Ctrl Pts',(0.241781714379012,-0.087720011286514,
-0.49898866032451));
#29433=CARTESIAN_POINT('Ctrl Pts',(0.205178141054117,0.155097157361885,
-0.491068205398723));
#29434=CARTESIAN_POINT('Ctrl Pts',(-0.0184495234412028,0.256540080441542,
-0.483147750472938));
#29435=CARTESIAN_POINT('Ctrl Pts',(-0.225260068255102,0.12414144931435,
-0.475227295547152));
#29436=CARTESIAN_POINT('Ctrl Pts',(-0.226741432650673,-0.121414663478844,
-0.467306840621366));
#29437=CARTESIAN_POINT('Ctrl Pts',(-0.0215433225451699,-0.256298815919768,
-0.45938638569558));
#29438=CARTESIAN_POINT('Ctrl Pts',(0.203291968690357,-0.157561331722472,
-0.451465930769794));
#29439=CARTESIAN_POINT('Ctrl Pts',(0.242822453618414,0.0847965436022809,
-0.443545475844009));
#29440=CARTESIAN_POINT('Ctrl Pts',(0.0610152830318996,0.24986062719984,
-0.435625020918222));
#29441=CARTESIAN_POINT('Ctrl Pts',(-0.176408571661025,0.187171615456717,
-0.427704565992437));
#29442=CARTESIAN_POINT('Ctrl Pts',(-0.253032388786235,-0.0461281694118899,
-0.419784111066651));
#29443=CARTESIAN_POINT('Ctrl Pts',(-0.0990119847176032,-0.237381180110053,
-0.411863656140865));
#29444=CARTESIAN_POINT('Ctrl Pts',(0.145259877725951,-0.212256367893173,
-0.403943201215079));
#29445=CARTESIAN_POINT('Ctrl Pts',(0.25712437710612,0.00634448468750714,
-0.396022746289293));
#29446=CARTESIAN_POINT('Ctrl Pts',(0.134614723864691,0.219162209121448,
-0.388102291363507));
#29447=CARTESIAN_POINT('Ctrl Pts',(-0.11059901597976,0.232209077024282,
-0.380181836437722));
#29448=CARTESIAN_POINT('Ctrl Pts',(-0.254999480386151,0.033592600241025,
-0.372261381511935));
#29449=CARTESIAN_POINT('Ctrl Pts',(-0.166962679189424,-0.195644221857049,
-0.36434092658615));
#29450=CARTESIAN_POINT('Ctrl Pts',(0.0732640345114102,-0.246547316017172,
-0.356420471660364));
#29451=CARTESIAN_POINT('Ctrl Pts',(0.246709075468843,-0.0727174660550607,
-0.348500016734578));
#29452=CARTESIAN_POINT('Ctrl Pts',(0.195273725240327,0.167395848272668,
-0.340579561808792));
#29453=CARTESIAN_POINT('Ctrl Pts',(-0.0341576376477591,0.254924407577,-0.332659106883006));
#29454=CARTESIAN_POINT('Ctrl Pts',(-0.232453612015502,0.110084131686205,
-0.324738651957221));
#29455=CARTESIAN_POINT('Ctrl Pts',(-0.218863343028437,-0.135100092030241,
-0.316818197031434));
#29456=CARTESIAN_POINT('Ctrl Pts',(-0.00577464009454566,-0.257137806088364,
-0.308897742105649));
#29457=CARTESIAN_POINT('Ctrl Pts',(0.212577765931518,-0.144789126731672,
-0.300977287179862));
#29458=CARTESIAN_POINT('Ctrl Pts',(0.237161170678426,0.0995378164850663,
-0.293056832254077));
#29459=CARTESIAN_POINT('Ctrl Pts',(0.0455672956274394,0.253133994867042,
-0.285136377328291));
#29460=CARTESIAN_POINT('Ctrl Pts',(-0.187562105615528,0.175993336024981,
-0.277215922402505));
#29461=CARTESIAN_POINT('Ctrl Pts',(-0.249724793930603,-0.0615688645712112,
-0.269295467476719));
#29462=CARTESIAN_POINT('Ctrl Pts',(-0.084258201720026,-0.243009780113768,
-0.261375012550933));
#29463=CARTESIAN_POINT('Ctrl Pts',(0.158011472529912,-0.202942288192858,
-0.253454557625148));
#29464=CARTESIAN_POINT('Ctrl Pts',(0.256250443060382,0.0221112690783347,
-0.245534102699361));
#29465=CARTESIAN_POINT('Ctrl Pts',(0.120911869802921,0.227009950283883,
-0.237613647773576));
#29466=CARTESIAN_POINT('Ctrl Pts',(-0.124640357031449,0.224984397651718,
-0.22969319284779));
#29467=CARTESIAN_POINT('Ctrl Pts',(-0.256580337582835,0.0178809440144413,
-0.221772737922004));
#29468=CARTESIAN_POINT('Ctrl Pts',(-0.154642068682266,-0.205521357463858,
-0.213852282996218));
#29469=CARTESIAN_POINT('Ctrl Pts',(0.0882556230412838,-0.241586718983118,
-0.205931828070432));
#29470=CARTESIAN_POINT('Ctrl Pts',(0.250706501180205,-0.0574408224581984,
-0.198011373144647));
#29471=CARTESIAN_POINT('Ctrl Pts',(0.184633252234903,0.179063563844805,
-0.190090918218861));
#29472=CARTESIAN_POINT('Ctrl Pts',(-0.0497369991668516,0.252347832796275,
-0.182170463293075));
#29473=CARTESIAN_POINT('Ctrl Pts',(-0.23877095476344,0.0956118671352282,
-0.174250008367289));
#29474=CARTESIAN_POINT('Ctrl Pts',(-0.210160277709292,-0.148276279355404,
-0.166329553441503));
#29475=CARTESIAN_POINT('Ctrl Pts',(0.0100158074287402,-0.257007551691304,
-0.158409098515717));
#29476=CARTESIAN_POINT('Ctrl Pts',(0.221062284030839,-0.131471158330418,
-0.150488643589931));
#29477=CARTESIAN_POINT('Ctrl Pts',(0.230605935914093,0.113903893563196,
-0.142568188664146));
#29478=CARTESIAN_POINT('Ctrl Pts',(0.0299475598214531,0.255453212845186,
-0.13464773373836));
#29479=CARTESIAN_POINT('Ctrl Pts',(-0.198008671586209,0.164151667438431,
-0.126727278812574));
#29480=CARTESIAN_POINT('Ctrl Pts',(-0.245475856005881,-0.0767774715160755,
-0.118806823886788));
#29481=CARTESIAN_POINT('Ctrl Pts',(-0.0691868957427056,-0.24772241328998,
-0.110886368961002));
#29482=CARTESIAN_POINT('Ctrl Pts',(0.170167610585507,-0.192863199035107,
-0.102965914035216));
#29483=CARTESIAN_POINT('Ctrl Pts',(0.254410332361144,0.0377946191841849,
-0.0950454591094304));
#29484=CARTESIAN_POINT('Ctrl Pts',(0.106753780372761,0.234002178088288,
-0.0871250041836445));
#29485=CARTESIAN_POINT('Ctrl Pts',(-0.138212881221763,0.216911349922406,
-0.0792045492578586));
#29486=CARTESIAN_POINT('Ctrl Pts',(-0.257192155654031,0.00210249804848441,
-0.0712840943320729));
#29487=CARTESIAN_POINT('Ctrl Pts',(-0.141742157498023,-0.214624967918095,
-0.063363639406287));
#29488=CARTESIAN_POINT('Ctrl Pts',(0.102921386109171,-0.235713292600032,
-0.055443184480501));
#29489=CARTESIAN_POINT('Ctrl Pts',(0.253745924148315,-0.0419518472751756,
-0.0475227295547153));
#29490=CARTESIAN_POINT('Ctrl Pts',(0.173321533153074,0.190064273543398,
-0.0396022746289292));
#29491=CARTESIAN_POINT('Ctrl Pts',(-0.0651758599354944,0.248804958958394,
-0.0316818197031436));
#29492=CARTESIAN_POINT('Ctrl Pts',(-0.244098679855147,0.0808079646592843,
-0.0237613647773576));
#29493=CARTESIAN_POINT('Ctrl Pts',(-0.200838287407273,-0.160948635674951,
-0.0158409098515717));
#29494=CARTESIAN_POINT('Ctrl Pts',(0.0261231005236458,-0.255800095598605,
-0.00792045492578602));
#29495=CARTESIAN_POINT('Ctrl Pts',(0.160601584503721,-0.163869943260562,
-0.0026401516419286));
#29496=CARTESIAN_POINT('Ctrl Pts',(0.193653104151514,-0.0996214127458699,
0.));
#29497=CARTESIAN_POINT('Ctrl Pts',(-0.0986179012119374,0.204792088618073,
-1.17464852262806));
#29498=CARTESIAN_POINT('Ctrl Pts',(-0.16656202641662,0.172073505236353,
-1.17200837098613));
#29499=CARTESIAN_POINT('Ctrl Pts',(-0.266177295204196,0.0342896334034012,
-1.16672806770228));
#29500=CARTESIAN_POINT('Ctrl Pts',(-0.173452084178045,-0.205124351144866,
-1.15880761277649));
#29501=CARTESIAN_POINT('Ctrl Pts',(0.0776013675721355,-0.256908479144051,
-1.1508871578507));
#29502=CARTESIAN_POINT('Ctrl Pts',(0.257804953624139,-0.0748439916648578,
-1.14296670292492));
#29503=CARTESIAN_POINT('Ctrl Pts',(0.203074034265681,0.175613484186487,
-1.13504624799913));
#29504=CARTESIAN_POINT('Ctrl Pts',(-0.036794585207094,0.265905798100996,
-1.12712579307335));
#29505=CARTESIAN_POINT('Ctrl Pts',(-0.243107585293851,0.113866785733275,
-1.11920533814756));
#29506=CARTESIAN_POINT('Ctrl Pts',(-0.22783176255635,-0.141989019123882,
-1.11128488322178));
#29507=CARTESIAN_POINT('Ctrl Pts',(-0.00487800918614132,-0.268405822095947,
-1.10336442829599));
#29508=CARTESIAN_POINT('Ctrl Pts',(0.22251972969843,-0.150172095122027,
-1.09544397337021));
#29509=CARTESIAN_POINT('Ctrl Pts',(0.247087436830596,0.10495020925552,-1.08752351844442));
#29510=CARTESIAN_POINT('Ctrl Pts',(0.0464291981955566,0.264406332440427,
-1.07960306351863));
#29511=CARTESIAN_POINT('Ctrl Pts',(-0.196549855663804,0.182851655946659,
-1.07168260859285));
#29512=CARTESIAN_POINT('Ctrl Pts',(-0.260369863488897,-0.0653765907044025,
-1.06376215366706));
#29513=CARTESIAN_POINT('Ctrl Pts',(-0.0868572934190015,-0.254012453329219,
-1.05584169874127));
#29514=CARTESIAN_POINT('Ctrl Pts',(0.165827432725362,-0.211110892307444,
-1.04792124381549));
#29515=CARTESIAN_POINT('Ctrl Pts',(0.267357073922758,0.0242226616622236,
-1.0400007888897));
#29516=CARTESIAN_POINT('Ctrl Pts',(0.125185234855463,0.237476721258427,
-1.03208033396392));
#29517=CARTESIAN_POINT('Ctrl Pts',(-0.131095510342261,0.234265891582874,
-1.02415987903813));
#29518=CARTESIAN_POINT('Ctrl Pts',(-0.267880008317113,0.0175168772476024,
-1.01623942411235));
#29519=CARTESIAN_POINT('Ctrl Pts',(-0.160486372757608,-0.21519912468331,
-1.00831896918656));
#29520=CARTESIAN_POINT('Ctrl Pts',(0.0931938878370631,-0.251756706089098,
-1.00039851426077));
#29521=CARTESIAN_POINT('Ctrl Pts',(0.26192600547804,-0.0588328756502444,
-0.992478059334988));
#29522=CARTESIAN_POINT('Ctrl Pts',(0.19190718727891,0.187718328863886,-0.984557604409201));
#29523=CARTESIAN_POINT('Ctrl Pts',(-0.0530389748994192,0.263160420203277,
-0.976637149483416));
#29524=CARTESIAN_POINT('Ctrl Pts',(-0.249639021799637,0.098726381382141,
-0.96871669455763));
#29525=CARTESIAN_POINT('Ctrl Pts',(-0.218687971190389,-0.155698782379805,
-0.960796239631844));
#29526=CARTESIAN_POINT('Ctrl Pts',(0.0116016583088355,-0.268201307074383,
-0.952875784706058));
#29527=CARTESIAN_POINT('Ctrl Pts',(0.231316137903588,-0.136232829859319,
-0.944955329780272));
#29528=CARTESIAN_POINT('Ctrl Pts',(0.240181205160686,0.119914670800206,
-0.937034874854487));
#29529=CARTESIAN_POINT('Ctrl Pts',(0.0301161691430373,0.266757485262614,
-0.9291144199287));
#29530=CARTESIAN_POINT('Ctrl Pts',(-0.207400373818482,0.170445371091411,
-0.921193965002915));
#29531=CARTESIAN_POINT('Ctrl Pts',(-0.255867214785822,-0.0812312008054323,
-0.913273510077128));
#29532=CARTESIAN_POINT('Ctrl Pts',(-0.0711058324167257,-0.258863864189515,
-0.905353055151343));
#29533=CARTESIAN_POINT('Ctrl Pts',(0.178469977144206,-0.200536796735162,
-0.897432600225557));
#29534=CARTESIAN_POINT('Ctrl Pts',(0.265366735685634,0.040583681181222,
-0.889512145299772));
#29535=CARTESIAN_POINT('Ctrl Pts',(0.110376262412427,0.244711299866933,
-0.881591690373985));
#29536=CARTESIAN_POINT('Ctrl Pts',(-0.145224441845548,0.225779540874117,
-0.8736712354482));
#29537=CARTESIAN_POINT('Ctrl Pts',(-0.268450083573173,0.00104509149768783,
-0.865750780522413));
#29538=CARTESIAN_POINT('Ctrl Pts',(-0.146977958536001,-0.224641980251412,
-0.857830325596628));
#29539=CARTESIAN_POINT('Ctrl Pts',(0.108467595522689,-0.245563271496795,
-0.849909870670841));
#29540=CARTESIAN_POINT('Ctrl Pts',(0.265042707682201,-0.0426485954185014,
-0.841989415745057));
#29541=CARTESIAN_POINT('Ctrl Pts',(0.180025946209632,0.199141151643779,
-0.834068960819269));
#29542=CARTESIAN_POINT('Ctrl Pts',(-0.069088164054453,0.259409647419421,
-0.826148505893485));
#29543=CARTESIAN_POINT('Ctrl Pts',(-0.255226993294282,0.0832209197296219,
-0.818228050967699));
#29544=CARTESIAN_POINT('Ctrl Pts',(-0.208721174240739,-0.168825386154603,
-0.810307596041912));
#29545=CARTESIAN_POINT('Ctrl Pts',(0.0280382835281578,-0.266983883864697,
-0.802387141116127));
#29546=CARTESIAN_POINT('Ctrl Pts',(0.239240269785266,-0.121781085968867,
-0.79446668619034));
#29547=CARTESIAN_POINT('Ctrl Pts',(0.232369834691432,0.134427673907422,
-0.786546231264555));
#29548=CARTESIAN_POINT('Ctrl Pts',(0.0136895209949644,0.268102847059877,
-0.77862577633877));
#29549=CARTESIAN_POINT('Ctrl Pts',(-0.217469072353946,0.157396766663733,
-0.770705321412982));
#29550=CARTESIAN_POINT('Ctrl Pts',(-0.250400138122595,-0.0967797004276667,
-0.762784866487198));
#29551=CARTESIAN_POINT('Ctrl Pts',(-0.0550863332596542,-0.262739482139038,
-0.754864411561411));
#29552=CARTESIAN_POINT('Ctrl Pts',(0.190439796175818,-0.189206827623098,
-0.746943956635626));
#29553=CARTESIAN_POINT('Ctrl Pts',(0.262376138612152,0.0567917377235466,
-0.739023501709839));
#29554=CARTESIAN_POINT('Ctrl Pts',(0.0951512399112054,0.251023467289502,
-0.731103046784055));
#29555=CARTESIAN_POINT('Ctrl Pts',(-0.158805968950592,0.216442148881283,
-0.723182591858267));
#29556=CARTESIAN_POINT('Ctrl Pts',(-0.268008274279125,-0.0154306352626495,
-0.715262136932482));
#29557=CARTESIAN_POINT('Ctrl Pts',(-0.132915531091811,-0.233238078326128,
-0.707341682006696));
#29558=CARTESIAN_POINT('Ctrl Pts',(0.123332449574351,-0.238444220874975,
-0.699421227080911));
#29559=CARTESIAN_POINT('Ctrl Pts',(0.267160368459267,-0.0263035570102677,
-0.691500772155124));
#29560=CARTESIAN_POINT('Ctrl Pts',(0.167466122404248,0.2098133395034,-0.68358031722934));
#29561=CARTESIAN_POINT('Ctrl Pts',(-0.0848769349889562,0.25468106622512,
-0.675659862303552));
#29562=CARTESIAN_POINT('Ctrl Pts',(-0.259852922254286,0.0674017683936514,
-0.667739407377768));
#29563=CARTESIAN_POINT('Ctrl Pts',(-0.197967631934649,-0.181315626168488,
-0.659818952451982));
#29564=CARTESIAN_POINT('Ctrl Pts',(0.0443692223455626,-0.264760102158791,
-0.651898497526195));
#29565=CARTESIAN_POINT('Ctrl Pts',(0.246262618845695,-0.106870305258026,
-0.64397804260041));
#29566=CARTESIAN_POINT('Ctrl Pts',(0.223682578544795,0.148433970647676,
-0.636057587674623));
#29567=CARTESIAN_POINT('Ctrl Pts',(-0.00278872789231205,0.26843763257678,
-0.628137132748838));
#29568=CARTESIAN_POINT('Ctrl Pts',(-0.226718051558245,0.143754877080107,
-0.620216677823052));
#29569=CARTESIAN_POINT('Ctrl Pts',(-0.243989213069241,-0.111963402469451,
-0.612296222897266));
#29570=CARTESIAN_POINT('Ctrl Pts',(-0.0388591938539432,-0.265624740262848,
-0.60437576797148));
#29571=CARTESIAN_POINT('Ctrl Pts',(0.201691778962022,-0.177163669768434,
-0.596455313045694));
#29572=CARTESIAN_POINT('Ctrl Pts',(0.258396551285464,0.0727857257328775,
-0.588534858119908));
#29573=CARTESIAN_POINT('Ctrl Pts',(0.0795675580846886,0.256389436769777,
-0.580614403194122));
#29574=CARTESIAN_POINT('Ctrl Pts',(-0.171788899109018,0.206288908401773,
-0.572693948268337));
#29575=CARTESIAN_POINT('Ctrl Pts',(-0.266556245182171,-0.0318481983959204,
-0.564773493342551));
#29576=CARTESIAN_POINT('Ctrl Pts',(-0.118352097094806,-0.240955018001172,
-0.556853038416764));
#29577=CARTESIAN_POINT('Ctrl Pts',(0.137732419162147,-0.230426388025387,
-0.54893258349098));
#29578=CARTESIAN_POINT('Ctrl Pts',(0.268271005496135,-0.00985937101321311,
-0.541012128565193));
#29579=CARTESIAN_POINT('Ctrl Pts',(0.154275058411882,0.219694665248599,
-0.533091673639407));
#29580=CARTESIAN_POINT('Ctrl Pts',(-0.100345774157302,0.248992500279537,
-0.525171218713622));
#29581=CARTESIAN_POINT('Ctrl Pts',(-0.263499371873178,0.0513285554942264,
-0.517250763787835));
#29582=CARTESIAN_POINT('Ctrl Pts',(-0.186467878256346,-0.193122422222952,
-0.509330308862051));
#29583=CARTESIAN_POINT('Ctrl Pts',(0.0605329175688147,-0.261538344181672,
-0.501409853936263));
#29584=CARTESIAN_POINT('Ctrl Pts',(0.252356715317872,-0.0915566918398557,
-0.493489399010479));
#29585=CARTESIAN_POINT('Ctrl Pts',(0.214152182121918,0.161880766242023,
-0.485568944084692));
#29586=CARTESIAN_POINT('Ctrl Pts',(-0.0192564650588239,0.267760579884571,
-0.477648489158906));
#29587=CARTESIAN_POINT('Ctrl Pts',(-0.235112448694224,0.129571123541048,
-0.469728034233121));
#29588=CARTESIAN_POINT('Ctrl Pts',(-0.23665860471357,-0.126725074084451,
-0.461807579307334));
#29589=CARTESIAN_POINT('Ctrl Pts',(-0.0224855801378355,-0.267508762982727,
-0.453887124381549));
#29590=CARTESIAN_POINT('Ctrl Pts',(0.212183512723307,-0.164452718174804,
-0.445966669455763));
#29591=CARTESIAN_POINT('Ctrl Pts',(0.25344297420487,0.0885053581026219,
-0.438046214529977));
#29592=CARTESIAN_POINT('Ctrl Pts',(0.0636839574475984,0.260788982034319,
-0.430125759604191));
#29593=CARTESIAN_POINT('Ctrl Pts',(-0.184124294976701,0.195358090659221,
-0.422205304678405));
#29594=CARTESIAN_POINT('Ctrl Pts',(-0.264099469503438,-0.0481457141881418,
-0.41428484975262));
#29595=CARTESIAN_POINT('Ctrl Pts',(-0.103342551377849,-0.247763711348939,
-0.406364394826833));
#29596=CARTESIAN_POINT('Ctrl Pts',(0.151613225609499,-0.22153999505048,
-0.398443939901048));
#29597=CARTESIAN_POINT('Ctrl Pts',(0.268370432401429,0.00662197850749817,
-0.390523484975262));
#29598=CARTESIAN_POINT('Ctrl Pts',(0.140502476108113,0.228747882600414,
-0.382603030049476));
#29599=CARTESIAN_POINT('Ctrl Pts',(-0.115436373928134,0.242365391838454,
-0.37468257512369));
#29600=CARTESIAN_POINT('Ctrl Pts',(-0.266152597367798,0.0350618667651702,
-0.366762120197904));
#29601=CARTESIAN_POINT('Ctrl Pts',(-0.174265259923113,-0.204201270247307,
-0.358841665272119));
#29602=CARTESIAN_POINT('Ctrl Pts',(0.0764684424035977,-0.2573307539006,
-0.350921210346332));
#29603=CARTESIAN_POINT('Ctrl Pts',(0.257499588355266,-0.0758979682438996,
-0.343000755420547));
#29604=CARTESIAN_POINT('Ctrl Pts',(0.203814568922633,0.17471737487029,-0.335080300494761));
#29605=CARTESIAN_POINT('Ctrl Pts',(-0.0356516176665625,0.266074241038927,
-0.327159845568975));
#29606=CARTESIAN_POINT('Ctrl Pts',(-0.242620622252893,0.114898969726894,
-0.319239390643189));
#29607=CARTESIAN_POINT('Ctrl Pts',(-0.228435944761169,-0.141009073210762,
-0.311318935717403));
#29608=CARTESIAN_POINT('Ctrl Pts',(-0.0060272101641153,-0.268384448737849,
-0.303398480791617));
#29609=CARTESIAN_POINT('Ctrl Pts',(0.221875450332839,-0.151121885001074,
-0.295478025865832));
#29610=CARTESIAN_POINT('Ctrl Pts',(0.247534079188182,0.103891381871452,
-0.287557570940045));
#29611=CARTESIAN_POINT('Ctrl Pts',(0.0475603090167235,0.264205519610968,
-0.27963711601426));
#29612=CARTESIAN_POINT('Ctrl Pts',(-0.195765659999584,0.183690897846301,
-0.271716661088473));
#29613=CARTESIAN_POINT('Ctrl Pts',(-0.26064720771634,-0.0642617514270981,
-0.263796206162689));
#29614=CARTESIAN_POINT('Ctrl Pts',(-0.0879434703292936,-0.253638493949533,
-0.255875751236902));
#29615=CARTESIAN_POINT('Ctrl Pts',(0.164922547152102,-0.211818537969172,
-0.247955296311117));
#29616=CARTESIAN_POINT('Ctrl Pts',(0.267458274400757,0.0230783674044562,
-0.24003484138533));
#29617=CARTESIAN_POINT('Ctrl Pts',(0.126200289317892,0.236938866718065,
-0.232114386459545));
#29618=CARTESIAN_POINT('Ctrl Pts',(-0.130091852385482,0.234824720864357,
-0.224193931533758));
#29619=CARTESIAN_POINT('Ctrl Pts',(-0.267802597784771,0.0186630172172313,
-0.216273476607973));
#29620=CARTESIAN_POINT('Ctrl Pts',(-0.161405772983488,-0.214510410063299,
-0.208353021682187));
#29621=CARTESIAN_POINT('Ctrl Pts',(0.0921157300759217,-0.252153191251809,
-0.200432566756401));
#29622=CARTESIAN_POINT('Ctrl Pts',(0.261671852684011,-0.0599531578222869,
-0.192512111830615));
#29623=CARTESIAN_POINT('Ctrl Pts',(0.192708705007432,0.186895410684992,
-0.18459165690483));
#29624=CARTESIAN_POINT('Ctrl Pts',(-0.051912386227186,0.263384972538599,
-0.176671201979044));
#29625=CARTESIAN_POINT('Ctrl Pts',(-0.249214271692021,0.0997937201232344,
-0.168750747053258));
#29626=CARTESIAN_POINT('Ctrl Pts',(-0.219352226487531,-0.154761558018521,
-0.160830292127472));
#29627=CARTESIAN_POINT('Ctrl Pts',(0.0104538768387219,-0.268248497299659,
-0.152909837201686));
#29628=CARTESIAN_POINT('Ctrl Pts',(0.230731062611456,-0.137221417924482,
-0.1449893822759));
#29629=CARTESIAN_POINT('Ctrl Pts',(0.240692132858562,0.11888579959552,-0.137068927350114));
#29630=CARTESIAN_POINT('Ctrl Pts',(0.0312574002866088,0.26662617508764,
-0.129148472424328));
#29631=CARTESIAN_POINT('Ctrl Pts',(-0.2066691358124,0.171331300694549,-0.121228017498543));
#29632=CARTESIAN_POINT('Ctrl Pts',(-0.25621243058265,-0.0801355494230467,
-0.113307562572757));
#29633=CARTESIAN_POINT('Ctrl Pts',(-0.0722129785435288,-0.258557247346171,
-0.105387107646971));
#29634=CARTESIAN_POINT('Ctrl Pts',(0.177610367976516,-0.201298611597657,
-0.097466652721185));
#29635=CARTESIAN_POINT('Ctrl Pts',(0.265537681302665,0.0394476727841362,
-0.0895461977953991));
#29636=CARTESIAN_POINT('Ctrl Pts',(0.111422956164521,0.244236919203158,
-0.0816257428696134));
#29637=CARTESIAN_POINT('Ctrl Pts',(-0.144258008962033,0.226398575765643,
-0.0737052879438273));
#29638=CARTESIAN_POINT('Ctrl Pts',(-0.2684411754341,0.00219445669347009,
-0.0657848330180417));
#29639=CARTESIAN_POINT('Ctrl Pts',(-0.147941648028013,-0.224012192436151,
-0.0578643780922557));
#29640=CARTESIAN_POINT('Ctrl Pts',(0.107422941396463,-0.246022874103948,
-0.0499439231664699));
#29641=CARTESIAN_POINT('Ctrl Pts',(0.264844213334459,-0.0437867288974735,
-0.042023468240684));
#29642=CARTESIAN_POINT('Ctrl Pts',(0.180902236187321,0.198377267254801,
-0.034103013314898));
#29643=CARTESIAN_POINT('Ctrl Pts',(-0.068026508843246,0.259687141183529,
-0.0261825583891124));
#29644=CARTESIAN_POINT('Ctrl Pts',(-0.254775019773046,0.0843423274804512,
-0.0182621034633263));
#29645=CARTESIAN_POINT('Ctrl Pts',(-0.209622512812183,-0.167988175359505,
-0.0103416485375405));
#29646=CARTESIAN_POINT('Ctrl Pts',(0.0272656675423015,-0.266988229730515,
-0.00242119361175477));
#29647=CARTESIAN_POINT('Ctrl Pts',(0.167625944932595,-0.171037254520151,
0.00285910967210262));
#29648=CARTESIAN_POINT('Ctrl Pts',(0.202123065428259,-0.103978634449024,
0.00549926131403122));
#29649=CARTESIAN_POINT('Ctrl Pts',(-0.10275048154209,0.213373895235262,
-1.16914926131403));
#29650=CARTESIAN_POINT('Ctrl Pts',(-0.173541803370507,0.179284240552571,
-1.1665091096721));
#29651=CARTESIAN_POINT('Ctrl Pts',(-0.277331447147971,0.0357265395106049,
-1.16122880638825));
#29652=CARTESIAN_POINT('Ctrl Pts',(-0.180720588805392,-0.21372008121374,
-1.15330835146246));
#29653=CARTESIAN_POINT('Ctrl Pts',(0.0808532506611131,-0.267674221615882,
-1.14538789653667));
#29654=CARTESIAN_POINT('Ctrl Pts',(0.268608262833421,-0.0779803269952925,
-1.13746744161088));
#29655=CARTESIAN_POINT('Ctrl Pts',(0.211583845864364,0.182972562219379,
-1.1295469866851));
#29656=CARTESIAN_POINT('Ctrl Pts',(-0.0383364612479987,0.277048572966425,
-1.12162653175931));
#29657=CARTESIAN_POINT('Ctrl Pts',(-0.253295001703547,0.118638370133228,
-1.11370607683353));
#29658=CARTESIAN_POINT('Ctrl Pts',(-0.237379046051068,-0.14793906490987,
-1.10578562190774));
#29659=CARTESIAN_POINT('Ctrl Pts',(-0.0050824220215922,-0.279653360395392,
-1.09786516698196));
#29660=CARTESIAN_POINT('Ctrl Pts',(0.231844412608142,-0.156465052473709,
-1.08994471205617));
#29661=CARTESIAN_POINT('Ctrl Pts',(0.257441628805129,0.109348144773157,
-1.08202425713039));
#29662=CARTESIAN_POINT('Ctrl Pts',(0.0483748124182258,0.275486272240229,
-1.0741038022046));
#29663=CARTESIAN_POINT('Ctrl Pts',(-0.204786271744744,0.190514049360174,
-1.06618334727882));
#29664=CARTESIAN_POINT('Ctrl Pts',(-0.271280655172714,-0.0681161948683243,
-1.05826289235303));
#29665=CARTESIAN_POINT('Ctrl Pts',(-0.0904970458159042,-0.264656837922096,
-1.05034243742724));
#29666=CARTESIAN_POINT('Ctrl Pts',(0.172776426551623,-0.21995748821254,
-1.04242198250146));
#29667=CARTESIAN_POINT('Ctrl Pts',(0.278560664459996,0.0252377116064939,
-1.03450152757567));
#29668=CARTESIAN_POINT('Ctrl Pts',(0.130431118542213,0.247428176471743,
-1.02658107264989));
#29669=CARTESIAN_POINT('Ctrl Pts',(-0.136589063954272,0.244082797070454,
-1.0186606177241));
#29670=CARTESIAN_POINT('Ctrl Pts',(-0.279105512405193,0.0182509214877408,
-1.01074016279831));
#29671=CARTESIAN_POINT('Ctrl Pts',(-0.167211549618656,-0.224217037849208,
-1.00281970787253));
#29672=CARTESIAN_POINT('Ctrl Pts',(0.09709917504185,-0.262306563658383,
-0.994899252946742));
#29673=CARTESIAN_POINT('Ctrl Pts',(0.272902007247412,-0.0612982656219496,
-0.986978798020957));
#29674=CARTESIAN_POINT('Ctrl Pts',(0.199949052473945,0.195584660066828,
-0.97905834309517));
#29675=CARTESIAN_POINT('Ctrl Pts',(-0.0552615716258469,0.27418815008641,
-0.971137888169384));
#29676=CARTESIAN_POINT('Ctrl Pts',(-0.260100137869332,0.102863507570724,
-0.963217433243599));
#29677=CARTESIAN_POINT('Ctrl Pts',(-0.227852084369397,-0.16222333540298,
-0.955296978317811));
#29678=CARTESIAN_POINT('Ctrl Pts',(0.0120878254684999,-0.279440275177697,
-0.947376523392029));
#29679=CARTESIAN_POINT('Ctrl Pts',(0.241009434047589,-0.141941662698782,
-0.93945606846624));
#29680=CARTESIAN_POINT('Ctrl Pts',(0.250245991694586,0.12493969165094,-0.931535613540455));
#29681=CARTESIAN_POINT('Ctrl Pts',(0.0313781863497569,0.277935950054195,
-0.92361515861467));
#29682=CARTESIAN_POINT('Ctrl Pts',(-0.216091480552406,0.177587879492844,
-0.915694703688883));
#29683=CARTESIAN_POINT('Ctrl Pts',(-0.266589323104498,-0.0846351919522501,
-0.907774248763098));
#29684=CARTESIAN_POINT('Ctrl Pts',(-0.0740855202907657,-0.269711547015759,
-0.899853793837311));
#29685=CARTESIAN_POINT('Ctrl Pts',(0.185948756432805,-0.208940285467685,
-0.891933338911526));
#29686=CARTESIAN_POINT('Ctrl Pts',(0.276486921155962,0.0422843391805672,
-0.884012883985739));
#29687=CARTESIAN_POINT('Ctrl Pts',(0.115001576532437,0.254965919889953,
-0.876092429059954));
#29688=CARTESIAN_POINT('Ctrl Pts',(-0.151310067928165,0.235240826077927,
-0.868171974134168));
#29689=CARTESIAN_POINT('Ctrl Pts',(-0.279699476648555,0.00108888602701205,
-0.860251519208383));
#29690=CARTESIAN_POINT('Ctrl Pts',(-0.153137065685387,-0.234055596009857,
-0.852331064282597));
#29691=CARTESIAN_POINT('Ctrl Pts',(0.113012927011266,-0.255853593366601,
-0.84441060935681));
#29692=CARTESIAN_POINT('Ctrl Pts',(0.276149314768311,-0.0444357835899101,
-0.836490154431025));
#29693=CARTESIAN_POINT('Ctrl Pts',(0.187569928337422,0.207486155908658,
-0.828569699505239));
#29694=CARTESIAN_POINT('Ctrl Pts',(-0.0719833015934706,0.270280201276306,
-0.820649244579453));
#29695=CARTESIAN_POINT('Ctrl Pts',(-0.265922273149663,0.086708289991059,
-0.812728789653667));
#29696=CARTESIAN_POINT('Ctrl Pts',(-0.217467629078588,-0.175900009133585,
-0.804808334727882));
#29697=CARTESIAN_POINT('Ctrl Pts',(0.0292132269976068,-0.278171835883225,
-0.796887879802095));
#29698=CARTESIAN_POINT('Ctrl Pts',(0.249265626449167,-0.126884318893871,
-0.78896742487631));
#29699=CARTESIAN_POINT('Ctrl Pts',(0.242107285969196,0.140060861738342,
-0.781046969950524));
#29700=CARTESIAN_POINT('Ctrl Pts',(0.0142631799807849,0.279337689199099,
-0.773126515024737));
#29701=CARTESIAN_POINT('Ctrl Pts',(-0.226582107612069,0.16399247366977,
-0.765206060098952));
#29702=CARTESIAN_POINT('Ctrl Pts',(-0.260893148750037,-0.100835251006521,
-0.757285605173166));
#29703=CARTESIAN_POINT('Ctrl Pts',(-0.0573947244796198,-0.273749572624627,
-0.749365150247381));
#29704=CARTESIAN_POINT('Ctrl Pts',(0.198420170388641,-0.197135534323977,
-0.741444695321594));
#29705=CARTESIAN_POINT('Ctrl Pts',(0.273371003197638,0.0591715938688031,
-0.733524240395808));
#29706=CARTESIAN_POINT('Ctrl Pts',(0.0991385498986852,0.261542598507859,
-0.725603785470023));
#29707=CARTESIAN_POINT('Ctrl Pts',(-0.165460728538161,0.22551215094065,
-0.717683330544237));
#29708=CARTESIAN_POINT('Ctrl Pts',(-0.279239153348675,-0.0160772555920675,
-0.709762875618451));
#29709=CARTESIAN_POINT('Ctrl Pts',(-0.138485352621285,-0.243011913328576,
-0.701842420692666));
#29710=CARTESIAN_POINT('Ctrl Pts',(0.128500692346879,-0.248436219132054,
-0.693921965766879));
#29711=CARTESIAN_POINT('Ctrl Pts',(0.278355716059682,-0.0274058068145916,
-0.686001510841094));
#29712=CARTESIAN_POINT('Ctrl Pts',(0.174483785474641,0.218605561495349,
-0.678081055915307));
#29713=CARTESIAN_POINT('Ctrl Pts',(-0.0884337005224793,0.265353469022279,
-0.670160600989522));
#29714=CARTESIAN_POINT('Ctrl Pts',(-0.270742051530451,0.070226237570728,
-0.662240146063736));
#29715=CARTESIAN_POINT('Ctrl Pts',(-0.206263459889676,-0.188913652298074,
-0.65431969113795));
#29716=CARTESIAN_POINT('Ctrl Pts',(0.0462285133391461,-0.275854866668525,
-0.646399236212164));
#29717=CARTESIAN_POINT('Ctrl Pts',(0.256582246846158,-0.111348702343739,
-0.638478781286378));
#29718=CARTESIAN_POINT('Ctrl Pts',(0.23305599060216,0.154654091942965,-0.630558326360593));
#29719=CARTESIAN_POINT('Ctrl Pts',(-0.00290558945489154,0.279686503893515,
-0.622637871434806));
#29720=CARTESIAN_POINT('Ctrl Pts',(-0.236218665025435,0.149778921093253,
-0.614717416509021));
#29721=CARTESIAN_POINT('Ctrl Pts',(-0.254213574065653,-0.116655225648164,
-0.606796961583234));
#29722=CARTESIAN_POINT('Ctrl Pts',(-0.040487587261153,-0.276755737407606,
-0.59887650665745));
#29723=CARTESIAN_POINT('Ctrl Pts',(0.210143667191733,-0.184587708283807,
-0.590956051731662));
#29724=CARTESIAN_POINT('Ctrl Pts',(0.269224651377827,0.075835809488292,
-0.583035596805878));
#29725=CARTESIAN_POINT('Ctrl Pts',(0.0829018343308682,0.267133428785756,
-0.57511514188009));
#29726=CARTESIAN_POINT('Ctrl Pts',(-0.178987708013609,0.214933439209195,
-0.567194686954306));
#29727=CARTESIAN_POINT('Ctrl Pts',(-0.277726277013936,-0.0331827962389527,
-0.559274232028519));
#29728=CARTESIAN_POINT('Ctrl Pts',(-0.1233116383391,-0.251052231140024,
-0.551353777102734));
#29729=CARTESIAN_POINT('Ctrl Pts',(0.143504092248462,-0.240082399226187,
-0.543433322176948));
#29730=CARTESIAN_POINT('Ctrl Pts',(0.279512894309821,-0.0102725276735772,
-0.535512867251162));
#29731=CARTESIAN_POINT('Ctrl Pts',(0.160739950322895,0.228900963913328,
-0.527592412325376));
#29732=CARTESIAN_POINT('Ctrl Pts',(-0.104550760953819,0.25942652388342,
-0.51967195739959));
#29733=CARTESIAN_POINT('Ctrl Pts',(-0.274541305516346,0.0534794771443913,
-0.511751502473804));
#29734=CARTESIAN_POINT('Ctrl Pts',(-0.194281809362337,-0.201215211803566,
-0.503831047548019));
#29735=CARTESIAN_POINT('Ctrl Pts',(0.0630695477485025,-0.272498101015506,
-0.495910592622232));
#29736=CARTESIAN_POINT('Ctrl Pts',(0.262931716256731,-0.0953933723931974,
-0.487990137696447));
#29737=CARTESIAN_POINT('Ctrl Pts',(0.223126223189719,0.16866437512216,-0.480069682770661));
#29738=CARTESIAN_POINT('Ctrl Pts',(-0.0200634066764452,0.278981079327601,
-0.472149227844875));
#29739=CARTESIAN_POINT('Ctrl Pts',(-0.244964829133346,0.135000797767746,
-0.464228772919089));
#29740=CARTESIAN_POINT('Ctrl Pts',(-0.246575776776468,-0.132035484690058,
-0.456308317993303));
#29741=CARTESIAN_POINT('Ctrl Pts',(-0.0234278377305011,-0.278718710045685,
-0.448387863067518));
#29742=CARTESIAN_POINT('Ctrl Pts',(0.221075056756257,-0.171344104627135,
-0.440467408141731));
#29743=CARTESIAN_POINT('Ctrl Pts',(0.264063494791325,0.0922141726029629,
-0.432546953215946));
#29744=CARTESIAN_POINT('Ctrl Pts',(0.0663526318632972,0.271717336868797,
-0.42462649829016));
#29745=CARTESIAN_POINT('Ctrl Pts',(-0.191840018292377,0.203544565861725,
-0.416706043364374));
#29746=CARTESIAN_POINT('Ctrl Pts',(-0.275166550220641,-0.0501632589643939,
-0.408785588438588));
#29747=CARTESIAN_POINT('Ctrl Pts',(-0.107673118038096,-0.258146242587824,
-0.400865133512802));
#29748=CARTESIAN_POINT('Ctrl Pts',(0.157966573493047,-0.230823622207787,
-0.392944678587017));
#29749=CARTESIAN_POINT('Ctrl Pts',(0.279616487696737,0.00689947232748906,
-0.38502422366123));
#29750=CARTESIAN_POINT('Ctrl Pts',(0.146390228351534,0.23833355607938,-0.377103768735445));
#29751=CARTESIAN_POINT('Ctrl Pts',(-0.120273731876508,0.252521706652626,
-0.369183313809658));
#29752=CARTESIAN_POINT('Ctrl Pts',(-0.277305714349445,0.0365311332893155,
-0.361262858883874));
#29753=CARTESIAN_POINT('Ctrl Pts',(-0.181567840656802,-0.212758318637564,
-0.353342403958087));
#29754=CARTESIAN_POINT('Ctrl Pts',(0.0796728502957855,-0.268114191784028,
-0.345421949032302));
#29755=CARTESIAN_POINT('Ctrl Pts',(0.268290101241689,-0.0790784704327387,
-0.337501494106515));
#29756=CARTESIAN_POINT('Ctrl Pts',(0.212355412604938,0.182038901467912,
-0.32958103918073));
#29757=CARTESIAN_POINT('Ctrl Pts',(-0.0371455976853658,0.277224074500852,
-0.321660584254944));
#29758=CARTESIAN_POINT('Ctrl Pts',(-0.252787632490283,0.119713807767583,
-0.313740129329158));
#29759=CARTESIAN_POINT('Ctrl Pts',(-0.238008546493902,-0.146918054391284,
-0.305819674403372));
#29760=CARTESIAN_POINT('Ctrl Pts',(-0.0062797802336852,-0.279631091387335,
-0.297899219477586));
#29761=CARTESIAN_POINT('Ctrl Pts',(0.23117313473416,-0.157454643270477,
-0.2899787645518));
#29762=CARTESIAN_POINT('Ctrl Pts',(0.257906987697937,0.108244947257839,
-0.282058309626014));
#29763=CARTESIAN_POINT('Ctrl Pts',(0.0495533224060077,0.275277044354895,
-0.274137854700229));
#29764=CARTESIAN_POINT('Ctrl Pts',(-0.203969214383641,0.191388459667621,
-0.266217399774442));
#29765=CARTESIAN_POINT('Ctrl Pts',(-0.271569621502078,-0.0669546382829851,
-0.258296944848657));
#29766=CARTESIAN_POINT('Ctrl Pts',(-0.0916287389385613,-0.264267207785298,
-0.250376489922871));
#29767=CARTESIAN_POINT('Ctrl Pts',(0.171833621774292,-0.220694787745487,
-0.242456034997085));
#29768=CARTESIAN_POINT('Ctrl Pts',(0.278666105741132,0.0240454657305778,
-0.234535580071299));
#29769=CARTESIAN_POINT('Ctrl Pts',(0.131488708832863,0.246867783152248,
-0.226615125145514));
#29770=CARTESIAN_POINT('Ctrl Pts',(-0.135543347739516,0.244665044076997,
-0.218694670219728));
#29771=CARTESIAN_POINT('Ctrl Pts',(-0.279024857986706,0.0194450904200208,
-0.210774215293942));
#29772=CARTESIAN_POINT('Ctrl Pts',(-0.16816947728471,-0.22349946266274,
-0.202853760368156));
#29773=CARTESIAN_POINT('Ctrl Pts',(0.0959758371105592,-0.2627196635205,
-0.19493330544237));
#29774=CARTESIAN_POINT('Ctrl Pts',(0.272637204187818,-0.0624654931863752,
-0.187012850516584));
#29775=CARTESIAN_POINT('Ctrl Pts',(0.200784157779961,0.194727257525179,
-0.179092395590798));
#29776=CARTESIAN_POINT('Ctrl Pts',(-0.0540877732875199,0.274422112280922,
-0.171171940665012));
#29777=CARTESIAN_POINT('Ctrl Pts',(-0.259657588620603,0.103975573111241,
-0.163251485739227));
#29778=CARTESIAN_POINT('Ctrl Pts',(-0.22854417526577,-0.161246836681637,
-0.155331030813441));
#29779=CARTESIAN_POINT('Ctrl Pts',(0.0108919462487035,-0.279489442908015,
-0.147410575887655));
#29780=CARTESIAN_POINT('Ctrl Pts',(0.240399841192072,-0.142971677518545,
-0.139490120961869));
#29781=CARTESIAN_POINT('Ctrl Pts',(0.250778329803031,0.123867705627845,
-0.131569666036083));
#29782=CARTESIAN_POINT('Ctrl Pts',(0.0325672407517647,0.277799137330094,
-0.123649211110297));
#29783=CARTESIAN_POINT('Ctrl Pts',(-0.21532960003859,0.178510933950667,
-0.115728756184511));
#29784=CARTESIAN_POINT('Ctrl Pts',(-0.26694900515942,-0.0834936273300177,
-0.107808301258725));
#29785=CARTESIAN_POINT('Ctrl Pts',(-0.0752390613443519,-0.269392081402363,
-0.0998878463329399));
#29786=CARTESIAN_POINT('Ctrl Pts',(0.185053125367525,-0.209734024160208,
-0.0919673914071537));
#29787=CARTESIAN_POINT('Ctrl Pts',(0.276665030244187,0.0411007263840873,
-0.0840469364813679));
#29788=CARTESIAN_POINT('Ctrl Pts',(0.116092131956281,0.254471660318029,
-0.0761264815555821));
#29789=CARTESIAN_POINT('Ctrl Pts',(-0.150303136702303,0.235885801608879,
-0.0682060266297961));
#29790=CARTESIAN_POINT('Ctrl Pts',(-0.27969019521417,0.00228641533845606,
-0.0602855717040106));
#29791=CARTESIAN_POINT('Ctrl Pts',(-0.154141138558003,-0.233399416954208,
-0.0523651167782244));
#29792=CARTESIAN_POINT('Ctrl Pts',(0.111924496683754,-0.256332455607864,
-0.0444446618524387));
#29793=CARTESIAN_POINT('Ctrl Pts',(0.275942502520604,-0.045621610519772,
-0.0365242069266528));
#29794=CARTESIAN_POINT('Ctrl Pts',(0.188482939221567,0.206690260966205,
-0.0286037520008668));
#29795=CARTESIAN_POINT('Ctrl Pts',(-0.0708771577509975,0.270569323408663,
-0.0206832970750811));
#29796=CARTESIAN_POINT('Ctrl Pts',(-0.265451359690944,0.0878766903016184,
-0.0127628421492951));
#29797=CARTESIAN_POINT('Ctrl Pts',(-0.218406738217093,-0.17502771504406,
-0.00484238722350926));
#29798=CARTESIAN_POINT('Ctrl Pts',(0.0284082345609573,-0.278176363862425,
0.00307806770227645));
#29799=CARTESIAN_POINT('Ctrl Pts',(0.174650305361468,-0.178204565779739,
0.00835837098613384));
#29800=CARTESIAN_POINT('Ctrl Pts',(0.210593026705004,-0.108335856152178,
0.0109985226280624));
#29801=CARTESIAN_POINT('Ctrl Pts',(-0.106883061872243,0.221955701852451,
-1.16365));
#29802=CARTESIAN_POINT('Ctrl Pts',(-0.180521580324393,0.186494975868788,
-1.16100984835807));
#29803=CARTESIAN_POINT('Ctrl Pts',(-0.288485599091745,0.0371634456178085,
-1.15572954507421));
#29804=CARTESIAN_POINT('Ctrl Pts',(-0.187989093432738,-0.222315811282613,
-1.14780909014843));
#29805=CARTESIAN_POINT('Ctrl Pts',(0.0841051337500907,-0.278439964087712,
-1.13988863522264));
#29806=CARTESIAN_POINT('Ctrl Pts',(0.279411572042703,-0.0811166623257269,
-1.13196818029685));
#29807=CARTESIAN_POINT('Ctrl Pts',(0.220093657463047,0.190331640252271,
-1.12404772537107));
#29808=CARTESIAN_POINT('Ctrl Pts',(-0.0398783372889031,0.288191347831854,
-1.11612727044528));
#29809=CARTESIAN_POINT('Ctrl Pts',(-0.263482418113243,0.123409954533181,
-1.1082068155195));
#29810=CARTESIAN_POINT('Ctrl Pts',(-0.246926329545785,-0.153889110695858,
-1.10028636059371));
#29811=CARTESIAN_POINT('Ctrl Pts',(-0.005286834857043,-0.290900898694837,
-1.09236590566793));
#29812=CARTESIAN_POINT('Ctrl Pts',(0.241169095517854,-0.162758009825391,
-1.08444545074214));
#29813=CARTESIAN_POINT('Ctrl Pts',(0.267795820779662,0.113746080290794,
-1.07652499581635));
#29814=CARTESIAN_POINT('Ctrl Pts',(0.0503204266408948,0.286566212040031,
-1.06860454089057));
#29815=CARTESIAN_POINT('Ctrl Pts',(-0.213022687825685,0.198176442773689,
-1.06068408596478));
#29816=CARTESIAN_POINT('Ctrl Pts',(-0.282191446856532,-0.0708557990322463,
-1.052763631039));
#29817=CARTESIAN_POINT('Ctrl Pts',(-0.0941367982128068,-0.275301222514972,
-1.04484317611321));
#29818=CARTESIAN_POINT('Ctrl Pts',(0.179725420377883,-0.228804084117637,
-1.03692272118743));
#29819=CARTESIAN_POINT('Ctrl Pts',(0.289764254997235,0.0262527615507647,
-1.02900226626164));
#29820=CARTESIAN_POINT('Ctrl Pts',(0.135677002228963,0.257379631685058,
-1.02108181133585));
#29821=CARTESIAN_POINT('Ctrl Pts',(-0.142082617566283,0.253899702558034,
-1.01316135641007));
#29822=CARTESIAN_POINT('Ctrl Pts',(-0.290331016493273,0.0189849657278787,
-1.00524090148428));
#29823=CARTESIAN_POINT('Ctrl Pts',(-0.173936726479704,-0.233234951015106,
-0.997320446558496));
#29824=CARTESIAN_POINT('Ctrl Pts',(0.101004462246637,-0.272856421227669,
-0.989399991632712));
#29825=CARTESIAN_POINT('Ctrl Pts',(0.283878009016785,-0.0637636555936547,
-0.981479536706925));
#29826=CARTESIAN_POINT('Ctrl Pts',(0.207990917668981,0.203450991269769,
-0.973559081781138));
#29827=CARTESIAN_POINT('Ctrl Pts',(-0.0574841683522745,0.285215879969544,
-0.965638626855354));
#29828=CARTESIAN_POINT('Ctrl Pts',(-0.270561253939026,0.107000633759307,
-0.957718171929567));
#29829=CARTESIAN_POINT('Ctrl Pts',(-0.237016197548405,-0.168747888426155,
-0.949797717003782));
#29830=CARTESIAN_POINT('Ctrl Pts',(0.0125739926281641,-0.290679243281013,
-0.941877262077995));
#29831=CARTESIAN_POINT('Ctrl Pts',(0.250702730191592,-0.147650495538245,
-0.933956807152211));
#29832=CARTESIAN_POINT('Ctrl Pts',(0.260310778228486,0.129964712501675,
-0.926036352226424));
#29833=CARTESIAN_POINT('Ctrl Pts',(0.0326402035564766,0.289114414845776,
-0.918115897300638));
#29834=CARTESIAN_POINT('Ctrl Pts',(-0.224782587286331,0.184730387894277,
-0.910195442374853));
#29835=CARTESIAN_POINT('Ctrl Pts',(-0.277311431423173,-0.0880391830990681,
-0.902274987449066));
#29836=CARTESIAN_POINT('Ctrl Pts',(-0.0770652081648057,-0.280559229842002,
-0.894354532523281));
#29837=CARTESIAN_POINT('Ctrl Pts',(0.193427535721404,-0.217343774200207,
-0.886434077597494));
#29838=CARTESIAN_POINT('Ctrl Pts',(0.287607106626291,0.0439849971799122,
-0.878513622671709));
#29839=CARTESIAN_POINT('Ctrl Pts',(0.119626890652448,0.265220539912974,
-0.870593167745923));
#29840=CARTESIAN_POINT('Ctrl Pts',(-0.157395694010782,0.244702111281736,
-0.862672712820137));
#29841=CARTESIAN_POINT('Ctrl Pts',(-0.290948869723938,0.00113268055633667,
-0.854752257894351));
#29842=CARTESIAN_POINT('Ctrl Pts',(-0.159296172834772,-0.243469211768303,
-0.846831802968566));
#29843=CARTESIAN_POINT('Ctrl Pts',(0.117558258499843,-0.266143915236407,
-0.838911348042778));
#29844=CARTESIAN_POINT('Ctrl Pts',(0.287255921854422,-0.046222971761319,
-0.830990893116994));
#29845=CARTESIAN_POINT('Ctrl Pts',(0.195113910465212,0.215831160173538,
-0.823070438191208));
#29846=CARTESIAN_POINT('Ctrl Pts',(-0.0748784391324881,0.281150755133191,
-0.815149983265422));
#29847=CARTESIAN_POINT('Ctrl Pts',(-0.276617553005043,0.0901956602524961,
-0.807229528339636));
#29848=CARTESIAN_POINT('Ctrl Pts',(-0.226214083916436,-0.182974632112567,
-0.799309073413849));
#29849=CARTESIAN_POINT('Ctrl Pts',(0.0303881704670555,-0.289359787901752,
-0.791388618488065));
#29850=CARTESIAN_POINT('Ctrl Pts',(0.259290983113068,-0.131987551818876,
-0.783468163562277));
#29851=CARTESIAN_POINT('Ctrl Pts',(0.251844737246961,0.145694049569263,
-0.775547708636494));
#29852=CARTESIAN_POINT('Ctrl Pts',(0.0148368389666054,0.290572531338322,
-0.767627253710706));
#29853=CARTESIAN_POINT('Ctrl Pts',(-0.235695142870192,0.170588180675806,
-0.759706798784921));
#29854=CARTESIAN_POINT('Ctrl Pts',(-0.27138615937748,-0.104890801585375,
-0.751786343859135));
#29855=CARTESIAN_POINT('Ctrl Pts',(-0.0597031156995855,-0.284759663110216,
-0.743865888933349));
#29856=CARTESIAN_POINT('Ctrl Pts',(0.206400544601464,-0.205064241024857,
-0.735945434007563));
#29857=CARTESIAN_POINT('Ctrl Pts',(0.284365867783122,0.0615514500140597,
-0.728024979081777));
#29858=CARTESIAN_POINT('Ctrl Pts',(0.103125859886165,0.272061729726216,
-0.720104524155992));
#29859=CARTESIAN_POINT('Ctrl Pts',(-0.17211548812573,0.234582153000017,
-0.712184069230205));
#29860=CARTESIAN_POINT('Ctrl Pts',(-0.290470032418224,-0.0167238759214858,
-0.70426361430442));
#29861=CARTESIAN_POINT('Ctrl Pts',(-0.144055174150759,-0.252785748331024,
-0.696343159378634));
#29862=CARTESIAN_POINT('Ctrl Pts',(0.133668935119408,-0.258428217389133,
-0.688422704452848));
#29863=CARTESIAN_POINT('Ctrl Pts',(0.289551063660099,-0.0285080566189151,
-0.680502249527062));
#29864=CARTESIAN_POINT('Ctrl Pts',(0.181501448545034,0.227397783487298,
-0.672581794601277));
#29865=CARTESIAN_POINT('Ctrl Pts',(-0.0919904660560023,0.276025871819438,
-0.66466133967549));
#29866=CARTESIAN_POINT('Ctrl Pts',(-0.281631180806615,0.0730507067478044,
-0.656740884749705));
#29867=CARTESIAN_POINT('Ctrl Pts',(-0.214559287844702,-0.196511678427659,
-0.648820429823918));
#29868=CARTESIAN_POINT('Ctrl Pts',(0.0480878043327292,-0.286949631178259,
-0.640899974898133));
#29869=CARTESIAN_POINT('Ctrl Pts',(0.266901874846621,-0.115827099429452,
-0.632979519972346));
#29870=CARTESIAN_POINT('Ctrl Pts',(0.242429402659526,0.160874213238254,
-0.625059065046561));
#29871=CARTESIAN_POINT('Ctrl Pts',(-0.00302245101747099,0.29093537521025,
-0.617138610120775));
#29872=CARTESIAN_POINT('Ctrl Pts',(-0.245719278492625,0.155802965106398,
-0.609218155194989));
#29873=CARTESIAN_POINT('Ctrl Pts',(-0.264437935062065,-0.121347048826877,
-0.601297700269203));
#29874=CARTESIAN_POINT('Ctrl Pts',(-0.0421159806683627,-0.287886734552365,
-0.593377245343418));
#29875=CARTESIAN_POINT('Ctrl Pts',(0.218595555421444,-0.19201174679918,
-0.585456790417632));
#29876=CARTESIAN_POINT('Ctrl Pts',(0.280052751470189,0.0788858932437061,
-0.577536335491846));
#29877=CARTESIAN_POINT('Ctrl Pts',(0.086236110577048,0.277877420801736,
-0.56961588056606));
#29878=CARTESIAN_POINT('Ctrl Pts',(-0.186186516918199,0.223577970016616,
-0.561695425640274));
#29879=CARTESIAN_POINT('Ctrl Pts',(-0.288896308845701,-0.0345173940819846,
-0.553774970714489));
#29880=CARTESIAN_POINT('Ctrl Pts',(-0.128271179583394,-0.261149444278877,
-0.545854515788702));
#29881=CARTESIAN_POINT('Ctrl Pts',(0.149275765334778,-0.249738410426987,
-0.537934060862917));
#29882=CARTESIAN_POINT('Ctrl Pts',(0.290754783123506,-0.0106856843339418,
-0.530013605937131));
#29883=CARTESIAN_POINT('Ctrl Pts',(0.167204842233907,0.238107262578057,
-0.522093151011345));
#29884=CARTESIAN_POINT('Ctrl Pts',(-0.108755747750336,0.269860547487303,
-0.514172696085559));
#29885=CARTESIAN_POINT('Ctrl Pts',(-0.285583239159514,0.0556303987945563,
-0.506252241159773));
#29886=CARTESIAN_POINT('Ctrl Pts',(-0.202095740468328,-0.20930800138418,
-0.498331786233988));
#29887=CARTESIAN_POINT('Ctrl Pts',(0.06560617792819,-0.283457857849339,
-0.490411331308201));
#29888=CARTESIAN_POINT('Ctrl Pts',(0.27350671719559,-0.0992300529465394,
-0.482490876382416));
#29889=CARTESIAN_POINT('Ctrl Pts',(0.232100264257521,0.175447984002298,
-0.47457042145663));
#29890=CARTESIAN_POINT('Ctrl Pts',(-0.0208703482940667,0.29020157877063,
-0.466649966530844));
#29891=CARTESIAN_POINT('Ctrl Pts',(-0.254817209572468,0.140430471994444,
-0.458729511605058));
#29892=CARTESIAN_POINT('Ctrl Pts',(-0.256492948839367,-0.137345895295664,
-0.450809056679272));
#29893=CARTESIAN_POINT('Ctrl Pts',(-0.0243700953231664,-0.289928657108644,
-0.442888601753487));
#29894=CARTESIAN_POINT('Ctrl Pts',(0.229966600789207,-0.178235491079467,
-0.4349681468277));
#29895=CARTESIAN_POINT('Ctrl Pts',(0.274684015377781,0.0959229871033038,
-0.427047691901915));
#29896=CARTESIAN_POINT('Ctrl Pts',(0.069021306278996,0.282645691703275,
-0.419127236976129));
#29897=CARTESIAN_POINT('Ctrl Pts',(-0.199555741608052,0.211731041064228,
-0.411206782050343));
#29898=CARTESIAN_POINT('Ctrl Pts',(-0.286233630937844,-0.0521808037406457,
-0.403286327124557));
#29899=CARTESIAN_POINT('Ctrl Pts',(-0.112003684698342,-0.268528773826709,
-0.395365872198771));
#29900=CARTESIAN_POINT('Ctrl Pts',(0.164319921376595,-0.240107249365093,
-0.387445417272986));
#29901=CARTESIAN_POINT('Ctrl Pts',(0.290862542992046,0.0071769661474798,
-0.379524962347199));
#29902=CARTESIAN_POINT('Ctrl Pts',(0.152277980594956,0.247919229558346,
-0.371604507421414));
#29903=CARTESIAN_POINT('Ctrl Pts',(-0.125111089824882,0.262678021466798,
-0.363684052495627));
#29904=CARTESIAN_POINT('Ctrl Pts',(-0.288458831331091,0.0380003998134609,
-0.355763597569842));
#29905=CARTESIAN_POINT('Ctrl Pts',(-0.188870421390492,-0.221315367027822,
-0.347843142644056));
#29906=CARTESIAN_POINT('Ctrl Pts',(0.0828772581879734,-0.278897629667457,
-0.33992268771827));
#29907=CARTESIAN_POINT('Ctrl Pts',(0.279080614128112,-0.0822589726215777,
-0.332002232792485));
#29908=CARTESIAN_POINT('Ctrl Pts',(0.220896256287244,0.189360428065534,
-0.324081777866698));
#29909=CARTESIAN_POINT('Ctrl Pts',(-0.0386395777041695,0.288373907962778,
-0.316161322940913));
#29910=CARTESIAN_POINT('Ctrl Pts',(-0.262954642727673,0.124528645808272,
-0.308240868015126));
#29911=CARTESIAN_POINT('Ctrl Pts',(-0.247581148226634,-0.152827035571806,
-0.300320413089341));
#29912=CARTESIAN_POINT('Ctrl Pts',(-0.00653235030325454,-0.29087773403682,
-0.292399958163555));
#29913=CARTESIAN_POINT('Ctrl Pts',(0.240470819135481,-0.16378740153988,
-0.284479503237769));
#29914=CARTESIAN_POINT('Ctrl Pts',(0.268279896207693,0.112598512644225,
-0.276559048311983));
#29915=CARTESIAN_POINT('Ctrl Pts',(0.0515463357952915,0.286348569098821,
-0.268638593386197));
#29916=CARTESIAN_POINT('Ctrl Pts',(-0.212172768767697,0.199086021488941,
-0.260718138460411));
#29917=CARTESIAN_POINT('Ctrl Pts',(-0.282492035287816,-0.0696475251388723,
-0.252797683534626));
#29918=CARTESIAN_POINT('Ctrl Pts',(-0.0953140075478283,-0.274895921621062,
-0.24487722860884));
#29919=CARTESIAN_POINT('Ctrl Pts',(0.178744696396482,-0.229571037521802,
-0.236956773683054));
#29920=CARTESIAN_POINT('Ctrl Pts',(0.289873937081507,0.0250125640566995,
-0.229036318757268));
#29921=CARTESIAN_POINT('Ctrl Pts',(0.136777128347834,0.25679669958643,-0.221115863831482));
#29922=CARTESIAN_POINT('Ctrl Pts',(-0.140994843093548,0.254505367289637,
-0.213195408905696));
#29923=CARTESIAN_POINT('Ctrl Pts',(-0.290247118188642,0.0202271636228108,
-0.20527495397991));
#29924=CARTESIAN_POINT('Ctrl Pts',(-0.174933181585931,-0.232488515262181,
-0.197354499054125));
#29925=CARTESIAN_POINT('Ctrl Pts',(0.0998359441451969,-0.273286135789191,
-0.189434044128339));
#29926=CARTESIAN_POINT('Ctrl Pts',(0.283602555691625,-0.0649778285504636,
-0.181513589202553));
#29927=CARTESIAN_POINT('Ctrl Pts',(0.208859610552489,0.202559104365367,
-0.173593134276767));
#29928=CARTESIAN_POINT('Ctrl Pts',(-0.0562631603478542,0.285459252023246,
-0.165672679350981));
#29929=CARTESIAN_POINT('Ctrl Pts',(-0.270100905549183,0.108157426099247,
-0.157752224425195));
#29930=CARTESIAN_POINT('Ctrl Pts',(-0.23773612404401,-0.167732115344754,
-0.149831769499409));
#29931=CARTESIAN_POINT('Ctrl Pts',(0.0113300156586853,-0.290730388516371,
-0.141911314573624));
#29932=CARTESIAN_POINT('Ctrl Pts',(0.250068619772689,-0.148721937112609,
-0.133990859647838));
#29933=CARTESIAN_POINT('Ctrl Pts',(0.2608645267475,0.128849611660169,-0.126070404722052));
#29934=CARTESIAN_POINT('Ctrl Pts',(0.0338770812169207,0.288972099572548,
-0.118149949796266));
#29935=CARTESIAN_POINT('Ctrl Pts',(-0.223990064264781,0.185690567206784,
-0.11022949487048));
#29936=CARTESIAN_POINT('Ctrl Pts',(-0.277685579736189,-0.0868517052369887,
-0.102309039944694));
#29937=CARTESIAN_POINT('Ctrl Pts',(-0.078265144145175,-0.280226915458554,
-0.0943885850189086));
#29938=CARTESIAN_POINT('Ctrl Pts',(0.192495882758534,-0.218169436722758,
-0.0864681300931225));
#29939=CARTESIAN_POINT('Ctrl Pts',(0.287792379185709,0.0427537799840384,
-0.0785476751673367));
#29940=CARTESIAN_POINT('Ctrl Pts',(0.120761307748041,0.2647064014329,-0.0706272202415509));
#29941=CARTESIAN_POINT('Ctrl Pts',(-0.156348264442573,0.245373027452116,
-0.0627067653157649));
#29942=CARTESIAN_POINT('Ctrl Pts',(-0.290939214994239,0.00237837398344197,
-0.0547863103899793));
#29943=CARTESIAN_POINT('Ctrl Pts',(-0.160340629087994,-0.242786641472266,
-0.0468658554641933));
#29944=CARTESIAN_POINT('Ctrl Pts',(0.116426051971046,-0.26664203711178,
-0.0389454005384074));
#29945=CARTESIAN_POINT('Ctrl Pts',(0.287040791706749,-0.0474564921420706,
-0.0310249456126217));
#29946=CARTESIAN_POINT('Ctrl Pts',(0.196063642255814,0.215003254677608,
-0.0231044906868355));
#29947=CARTESIAN_POINT('Ctrl Pts',(-0.0737278066587491,0.281451505633798,
-0.01518403576105));
#29948=CARTESIAN_POINT('Ctrl Pts',(-0.276127699608842,0.0914110531227855,
-0.00726358083526385));
#29949=CARTESIAN_POINT('Ctrl Pts',(-0.227190963622003,-0.182067254728615,
0.00065687409052195));
#29950=CARTESIAN_POINT('Ctrl Pts',(0.029550801579613,-0.289364497994335,
0.00857732901630768));
#29951=CARTESIAN_POINT('Ctrl Pts',(0.181674665790342,-0.185371877039327,
0.0138576323001651));
#29952=CARTESIAN_POINT('Ctrl Pts',(0.219062987981749,-0.112693077855332,
0.0164977839420937));
#29953=CARTESIAN_POINT('',(-0.204509257318296,-0.138028148648276,-2.52416797836347E-16));
#29954=CARTESIAN_POINT('Ctrl Pts',(-0.204513561691918,-0.138033045165328,
7.97972798949331E-17));
#29955=CARTESIAN_POINT('Ctrl Pts',(-0.200458969367413,-0.14343453541669,
1.13314958597239E-16));
#29956=CARTESIAN_POINT('Ctrl Pts',(-0.196176350401663,-0.14864871991259,
5.9397114527851E-16));
#29957=CARTESIAN_POINT('Ctrl Pts',(-0.191667490565443,-0.153657468545478,
4.5102810375397E-16));
#29958=CARTESIAN_POINT('Ctrl Pts',(-0.183969917901797,-0.162208456590365,
2.03524801489296E-16));
#29959=CARTESIAN_POINT('Ctrl Pts',(-0.175613388124977,-0.170161490060188,
-1.5271922467326E-16));
#29960=CARTESIAN_POINT('Ctrl Pts',(-0.166688955232968,-0.177488068326711,
-2.51534904016637E-16));
#29961=CARTESIAN_POINT('Ctrl Pts',(-0.161662997196323,-0.181614165230046,
-3.07184765890441E-16));
#29962=CARTESIAN_POINT('Ctrl Pts',(-0.156453755055607,-0.18554289472659,
-4.44006003611873E-16));
#29963=CARTESIAN_POINT('Ctrl Pts',(-0.151098143157478,-0.1892536575405,
-3.72965547335014E-16));
#29964=CARTESIAN_POINT('Ctrl Pts',(-0.143555040089887,-0.194480075529169,
-2.72908729578602E-16));
#29965=CARTESIAN_POINT('Ctrl Pts',(-0.135714281411093,-0.199281170935203,
-2.35696859612518E-16));
#29966=CARTESIAN_POINT('Ctrl Pts',(-0.127621690156068,-0.203642056189206,
-3.22658566531686E-16));
#29967=CARTESIAN_POINT('Ctrl Pts',(-0.122072656842052,-0.206632284756358,
-3.82287601723413E-16));
#29968=CARTESIAN_POINT('Ctrl Pts',(-0.1164051378392,-0.209415418232596,
-3.70654868758527E-16));
#29969=CARTESIAN_POINT('Ctrl Pts',(-0.110633357581212,-0.211984946769715,
-3.81639164714898E-16));
#29970=CARTESIAN_POINT('Ctrl Pts',(-0.106100414669248,-0.214002959522939,
-3.90265824821965E-16));
#29971=CARTESIAN_POINT('Ctrl Pts',(-0.101501721030156,-0.21588944006491,
-4.94020418234288E-16));
#29972=CARTESIAN_POINT('Ctrl Pts',(-0.0968614704712326,-0.217634943816702,
-4.9960036108132E-16));
#29973=CARTESIAN_POINT('Ctrl Pts',(-0.0826821613338624,-0.222968715556572,
-5.16651107283974E-16));
#29974=CARTESIAN_POINT('Ctrl Pts',(-0.0680806317286739,-0.227006644225286,
-3.92788537165852E-16));
#29975=CARTESIAN_POINT('Ctrl Pts',(-0.0532579471984103,-0.229671072551787,
-4.04190569902596E-16));
#29976=CARTESIAN_POINT('Ctrl Pts',(-0.0416423014901125,-0.231759024662797,
-4.13125656684887E-16));
#29977=CARTESIAN_POINT('Ctrl Pts',(-0.0298901490078552,-0.233002671776119,
-2.53258607599116E-16));
#29978=CARTESIAN_POINT('Ctrl Pts',(-0.0180992304553012,-0.233341545130159,
-2.41126563160776E-16));
#29979=CARTESIAN_POINT('Ctrl Pts',(-0.014418495701006,-0.2334473301821,
-2.37339340188637E-16));
#29980=CARTESIAN_POINT('Ctrl Pts',(-0.0107362607675731,-0.233464579565444,
-5.5259238222526E-16));
#29981=CARTESIAN_POINT('Ctrl Pts',(-0.00706437366680782,-0.233391940295786,
-5.25621213220973E-16));
#29982=CARTESIAN_POINT('Ctrl Pts',(0.00313705648947054,-0.233190130050622,
-4.50688490814264E-16));
#29983=CARTESIAN_POINT('Ctrl Pts',(0.0132783977524309,-0.232296137191171,
-2.4101113858591E-16));
#29984=CARTESIAN_POINT('Ctrl Pts',(0.0232964001888359,-0.230679356207016,
-1.64798730217797E-16));
#29985=CARTESIAN_POINT('Ctrl Pts',(0.0344038527887266,-0.228886751517617,
-8.36100771269679E-17));
#29986=CARTESIAN_POINT('Ctrl Pts',(0.0453601005161749,-0.226205689418119,
-9.88173003853937E-17));
#29987=CARTESIAN_POINT('Ctrl Pts',(0.0560899933785598,-0.222695008049497,
-1.50053580671994E-16));
#29988=CARTESIAN_POINT('Ctrl Pts',(0.0605383051258949,-0.221239578310032,
-1.71294701194979E-16));
#29989=CARTESIAN_POINT('Ctrl Pts',(0.0649476163018993,-0.219641368744839,
-2.82468155353174E-16));
#29990=CARTESIAN_POINT('Ctrl Pts',(0.0693120640699186,-0.217903830273792,
-3.35668992601512E-16));
#29991=CARTESIAN_POINT('Ctrl Pts',(0.0726902936253035,-0.216558916981549,
-3.76848232293759E-16));
#29992=CARTESIAN_POINT('Ctrl Pts',(0.0760395849689661,-0.215131185718671,
-1.66001976769033E-16));
#29993=CARTESIAN_POINT('Ctrl Pts',(0.0793492735533264,-0.21362643030463,
-1.39645239816133E-16));
#29994=CARTESIAN_POINT('Ctrl Pts',(0.0918661238439923,-0.2079356235228,
-3.99671818414834E-17));
#29995=CARTESIAN_POINT('Ctrl Pts',(0.103852408746883,-0.201132648912409,
1.2723644335876E-17));
#29996=CARTESIAN_POINT('Ctrl Pts',(0.115173520844875,-0.193329455672931,
-1.16226472890446E-16));
#29997=CARTESIAN_POINT('Ctrl Pts',(0.125337633549786,-0.186323736194337,
-2.31998096159875E-16));
#29998=CARTESIAN_POINT('Ctrl Pts',(0.134965897482742,-0.178510810996301,
1.26912968512929E-16));
#29999=CARTESIAN_POINT('Ctrl Pts',(0.14394042956759,-0.169952142766193,
2.51101223147643E-16));
#30000=CARTESIAN_POINT('Ctrl Pts',(0.146996369828429,-0.167037809341757,
2.93388874879624E-16));
#30001=CARTESIAN_POINT('Ctrl Pts',(0.149970279662056,-0.164042501082029,
3.04623096677509E-16));
#30002=CARTESIAN_POINT('Ctrl Pts',(0.15285458649515,-0.160973061898707,
2.53269627492614E-16));
#30003=CARTESIAN_POINT('Ctrl Pts',(0.162422461331181,-0.150791062679389,
8.2918969955242E-17));
#30004=CARTESIAN_POINT('Ctrl Pts',(0.171020780523213,-0.139782655946406,
-2.2682857248612E-16));
#30005=CARTESIAN_POINT('Ctrl Pts',(0.178487646579902,-0.128046791389447,
-3.42174205636425E-16));
#30006=CARTESIAN_POINT('Ctrl Pts',(0.184248186336547,-0.118992803565679,
-4.31161084532231E-16));
#30007=CARTESIAN_POINT('Ctrl Pts',(0.189334785443673,-0.1095050565137,2.58952566004617E-17));
#30008=CARTESIAN_POINT('Ctrl Pts',(0.193653104151514,-0.0996214127458699,
0.));
#30009=CARTESIAN_POINT('Ctrl Pts',(-0.246160120813712,0.000192360259597545,
-0.00472127808698222));
#30010=CARTESIAN_POINT('Ctrl Pts',(-0.24582237483402,-0.0486236404045207,
-0.00314751872465485));
#30011=CARTESIAN_POINT('Ctrl Pts',(-0.231427963796332,-0.0976359744578188,
-0.0015737593623275));
#30012=CARTESIAN_POINT('Ctrl Pts',(-0.204513561691922,-0.138033045165322,
-1.45716771982052E-16));
#30013=CARTESIAN_POINT('',(-0.126471106027292,-0.177287929553124,-1.16365));
#30014=CARTESIAN_POINT('Ctrl Pts',(-0.126742452678739,-0.177514072314448,
-1.16365));
#30015=CARTESIAN_POINT('Ctrl Pts',(-0.131861338221367,-0.174371803129766,
-1.16365));
#30016=CARTESIAN_POINT('Ctrl Pts',(-0.136831729034579,-0.171012070470409,
-1.16365));
#30017=CARTESIAN_POINT('Ctrl Pts',(-0.141637451548538,-0.167437627045634,
-1.16365));
#30018=CARTESIAN_POINT('Ctrl Pts',(-0.150897109985627,-0.160550395184039,
-1.16365));
#30019=CARTESIAN_POINT('Ctrl Pts',(-0.159546413429048,-0.152867380212311,
-1.16365));
#30020=CARTESIAN_POINT('Ctrl Pts',(-0.16755538633808,-0.144504071864687,
-1.16365));
#30021=CARTESIAN_POINT('Ctrl Pts',(-0.17090995218102,-0.141001092289706,
-1.16365));
#30022=CARTESIAN_POINT('Ctrl Pts',(-0.174151378696826,-0.137378738244585,
-1.16365));
#30023=CARTESIAN_POINT('Ctrl Pts',(-0.177268691376915,-0.133655610415481,
-1.16365));
#30024=CARTESIAN_POINT('Ctrl Pts',(-0.186038283781417,-0.12318174498015,
-1.16365));
#30025=CARTESIAN_POINT('Ctrl Pts',(-0.193847100730409,-0.111893260660668,
-1.16365));
#30026=CARTESIAN_POINT('Ctrl Pts',(-0.200640170312477,-0.0999687378212474,
-1.16365));
#30027=CARTESIAN_POINT('Ctrl Pts',(-0.203365214294673,-0.0951852082531265,
-1.16365));
#30028=CARTESIAN_POINT('Ctrl Pts',(-0.205927329765095,-0.0902963247364379,
-1.16365));
#30029=CARTESIAN_POINT('Ctrl Pts',(-0.208311993322315,-0.0853347291837548,
-1.16365));
#30030=CARTESIAN_POINT('Ctrl Pts',(-0.214711771281109,-0.072019177913485,
-1.16365));
#30031=CARTESIAN_POINT('Ctrl Pts',(-0.219855302751287,-0.0581522607815734,
-1.16365));
#30032=CARTESIAN_POINT('Ctrl Pts',(-0.223672726060924,-0.0439462398011037,
-1.16365));
#30033=CARTESIAN_POINT('Ctrl Pts',(-0.226338842024177,-0.0340246523222635,
-1.16365));
#30034=CARTESIAN_POINT('Ctrl Pts',(-0.228357386302339,-0.0239367220668382,
-1.16365));
#30035=CARTESIAN_POINT('Ctrl Pts',(-0.229690730670339,-0.013748733749612,
-1.16365));
#30036=CARTESIAN_POINT('Ctrl Pts',(-0.230229670333924,-0.00963073458295048,
-1.16365));
#30037=CARTESIAN_POINT('Ctrl Pts',(-0.230656273552338,-0.00549607418239393,
-1.16365));
#30038=CARTESIAN_POINT('Ctrl Pts',(-0.230967088650693,-0.00136420452645389,
-1.16365));
#30039=CARTESIAN_POINT('Ctrl Pts',(-0.231742593736289,0.00894509495149809,
-1.16365));
#30040=CARTESIAN_POINT('Ctrl Pts',(-0.231801493177623,0.0192593571944351,
-1.16365));
#30041=CARTESIAN_POINT('Ctrl Pts',(-0.231115915127983,0.0295095610734199,
-1.16365));
#30042=CARTESIAN_POINT('Ctrl Pts',(-0.230457433078469,0.0393546476565208,
-1.16365));
#30043=CARTESIAN_POINT('Ctrl Pts',(-0.229112221005407,0.0491408939728083,
-1.16365));
#30044=CARTESIAN_POINT('Ctrl Pts',(-0.227122783666268,0.0588215211318158,
-1.16365));
#30045=CARTESIAN_POINT('Ctrl Pts',(-0.22602341141252,0.0641710803705567,
-1.16365));
#30046=CARTESIAN_POINT('Ctrl Pts',(-0.224727103207668,0.0694883890758916,
-1.16365));
#30047=CARTESIAN_POINT('Ctrl Pts',(-0.223239600591205,0.074765365573958,
-1.16365));
#30048=CARTESIAN_POINT('Ctrl Pts',(-0.222045632550997,0.0790010161320732,
-1.16365));
#30049=CARTESIAN_POINT('Ctrl Pts',(-0.220727846656266,0.083211665253357,
-1.16365));
#30050=CARTESIAN_POINT('Ctrl Pts',(-0.219295202918089,0.0873767379509316,
-1.16365));
#30051=CARTESIAN_POINT('Ctrl Pts',(-0.21444725735436,0.101470992627617,
-1.16365));
#30052=CARTESIAN_POINT('Ctrl Pts',(-0.208276894357113,0.115087695452192,
-1.16365));
#30053=CARTESIAN_POINT('Ctrl Pts',(-0.200926527149074,0.128072014981204,
-1.16365));
#30054=CARTESIAN_POINT('Ctrl Pts',(-0.197308721049431,0.134462818197185,
-1.16365));
#30055=CARTESIAN_POINT('Ctrl Pts',(-0.193404247750143,0.140700343051493,
-1.16365));
#30056=CARTESIAN_POINT('Ctrl Pts',(-0.189225861417297,0.146764841991167,
-1.16365));
#30057=CARTESIAN_POINT('Ctrl Pts',(-0.18619672096879,0.151161328475361,
-1.16365));
#30058=CARTESIAN_POINT('Ctrl Pts',(-0.183023566145792,0.155466860400186,
-1.16365));
#30059=CARTESIAN_POINT('Ctrl Pts',(-0.179710475436982,0.159673387333553,
-1.16365));
#30060=CARTESIAN_POINT('Ctrl Pts',(-0.176874734026243,0.163273838896385,
-1.16365));
#30061=CARTESIAN_POINT('Ctrl Pts',(-0.17394079312019,0.166796008550431,
-1.16365));
#30062=CARTESIAN_POINT('Ctrl Pts',(-0.170917645960835,0.170229306991485,
-1.16365));
#30063=CARTESIAN_POINT('Ctrl Pts',(-0.160759806788243,0.181765263250785,
-1.16365));
#30064=CARTESIAN_POINT('Ctrl Pts',(-0.149580565015023,0.192322357430371,
-1.16365));
#30065=CARTESIAN_POINT('Ctrl Pts',(-0.137500883169785,0.201728680603211,
-1.16365));
#30066=CARTESIAN_POINT('Ctrl Pts',(-0.127855257975516,0.209239629065579,
-1.16365));
#30067=CARTESIAN_POINT('Ctrl Pts',(-0.117634401071449,0.216016836489331,
-1.16365));
#30068=CARTESIAN_POINT('Ctrl Pts',(-0.106883061872243,0.221955701852451,
-1.16365));
#30069=CARTESIAN_POINT('Ctrl Pts',(-0.126742452678738,-0.177514072314449,
-1.16365));
#30070=CARTESIAN_POINT('Ctrl Pts',(-0.0727848118484482,-0.215552950999294,
-1.16122880638825));
#30071=CARTESIAN_POINT('Ctrl Pts',(0.0791223892213512,-0.241320543762611,
-1.15616746113456));
#30072=CARTESIAN_POINT('Ctrl Pts',(0.247001644414856,-0.0717076563344237,
-1.14846596423895));
#30073=CARTESIAN_POINT('Ctrl Pts',(0.194564222666998,0.168254406153596,
-1.14054550931316));
#30074=CARTESIAN_POINT('Ctrl Pts',(-0.0352527091661894,0.254763023235567,
-1.13262505438738));
#30075=CARTESIAN_POINT('Ctrl Pts',(-0.196026712503706,0.136283234411974,
-1.12618290529268));
#30076=CARTESIAN_POINT('Ctrl Pts',(-0.21753268144054,0.0319805760390736,
-1.12238090783991));
#30077=CARTESIAN_POINT('Ctrl Pts',(-0.217441534898734,7.07751596318099E-5,
-1.12121906202908));
#30078=CARTESIAN_POINT('Origin',(-2.26018097944867E-17,0.,-1.16365));
#30079=CARTESIAN_POINT('',(-0.24635,-3.01691738969951E-17,-1.16365));
#30080=CARTESIAN_POINT('Origin',(0.,0.,-1.16365));
#30081=CARTESIAN_POINT('Origin',(0.,0.,-1.16365));
#30082=CARTESIAN_POINT('',(0.126471106027295,-0.177287929553122,-1.16365));
#30083=CARTESIAN_POINT('Ctrl Pts',(0.10714206075237,0.222259968661296,-1.16365));
#30084=CARTESIAN_POINT('Ctrl Pts',(0.113071151342837,0.219025513962988,
-1.16365));
#30085=CARTESIAN_POINT('Ctrl Pts',(0.118847726774383,0.21553843574513,-1.16365));
#30086=CARTESIAN_POINT('Ctrl Pts',(0.12445358873384,0.211797890271589,-1.16365));
#30087=CARTESIAN_POINT('Ctrl Pts',(0.134023975740716,0.205411991357647,
-1.16365));
#30088=CARTESIAN_POINT('Ctrl Pts',(0.143097537518038,0.198287893018338,
-1.16365));
#30089=CARTESIAN_POINT('Ctrl Pts',(0.151632957908753,0.190511595485141,
-1.16365));
#30090=CARTESIAN_POINT('Ctrl Pts',(0.156439835694909,0.18613223159212,-1.16365));
#30091=CARTESIAN_POINT('Ctrl Pts',(0.161077798201613,0.181543071307519,
-1.16365));
#30092=CARTESIAN_POINT('Ctrl Pts',(0.165521144850447,0.176777677610949,
-1.16365));
#30093=CARTESIAN_POINT('Ctrl Pts',(0.171779371002945,0.170065864687989,
-1.16365));
#30094=CARTESIAN_POINT('Ctrl Pts',(0.177659573392144,0.162998247969616,
-1.16365));
#30095=CARTESIAN_POINT('Ctrl Pts',(0.183140420688034,0.155618028761713,
-1.16365));
#30096=CARTESIAN_POINT('Ctrl Pts',(0.186898597060763,0.15055746714499,-1.16365));
#30097=CARTESIAN_POINT('Ctrl Pts',(0.190468900412591,0.14534983118815,-1.16365));
#30098=CARTESIAN_POINT('Ctrl Pts',(0.193842840317149,0.140008259503939,
-1.16365));
#30099=CARTESIAN_POINT('Ctrl Pts',(0.196492609601869,0.135813184019093,
-1.16365));
#30100=CARTESIAN_POINT('Ctrl Pts',(0.199021686516466,0.131534101113879,
-1.16365));
#30101=CARTESIAN_POINT('Ctrl Pts',(0.201417240773586,0.127193592262789,
-1.16365));
#30102=CARTESIAN_POINT('Ctrl Pts',(0.208737384344553,0.113930211620668,
-1.16365));
#30103=CARTESIAN_POINT('Ctrl Pts',(0.214835996804749,0.100062396156116,
-1.16365));
#30104=CARTESIAN_POINT('Ctrl Pts',(0.219607275101183,0.0857779314832026,
-1.16365));
#30105=CARTESIAN_POINT('Ctrl Pts',(0.223346238611081,0.0745840566236364,
-1.16365));
#30106=CARTESIAN_POINT('Ctrl Pts',(0.22626935672672,0.0631335084732036,
-1.16365));
#30107=CARTESIAN_POINT('Ctrl Pts',(0.228302715464478,0.0515143004487872,
-1.16365));
#30108=CARTESIAN_POINT('Ctrl Pts',(0.228937463003728,0.0478871668965153,
-1.16365));
#30109=CARTESIAN_POINT('Ctrl Pts',(0.229484813783808,0.0442457986424989,
-1.16365));
#30110=CARTESIAN_POINT('Ctrl Pts',(0.229941722688576,0.0406017253371934,
-1.16365));
#30111=CARTESIAN_POINT('Ctrl Pts',(0.231211130326128,0.030477574905268,
-1.16365));
#30112=CARTESIAN_POINT('Ctrl Pts',(0.231786917854907,0.0203132046570649,
-1.16365));
#30113=CARTESIAN_POINT('Ctrl Pts',(0.231629690263984,0.010166797456069,
-1.16365));
#30114=CARTESIAN_POINT('Ctrl Pts',(0.231455364231173,-0.00108302774480546,
-1.16365));
#30115=CARTESIAN_POINT('Ctrl Pts',(0.230380067272138,-0.0123111726630605,
-1.16365));
#30116=CARTESIAN_POINT('Ctrl Pts',(0.228451201638814,-0.0234347970229404,
-1.16365));
#30117=CARTESIAN_POINT('Ctrl Pts',(0.227651547930891,-0.0280463403628394,
-1.16365));
#30118=CARTESIAN_POINT('Ctrl Pts',(0.226704986161851,-0.0326398516094958,
-1.16365));
#30119=CARTESIAN_POINT('Ctrl Pts',(0.225614086959102,-0.0372090320414421,
-1.16365));
#30120=CARTESIAN_POINT('Ctrl Pts',(0.224769694305267,-0.0407457312901538,
-1.16365));
#30121=CARTESIAN_POINT('Ctrl Pts',(0.223839179533421,-0.0442657206832852,
-1.16365));
#30122=CARTESIAN_POINT('Ctrl Pts',(0.222826740250488,-0.0477576124712794,
-1.16365));
#30123=CARTESIAN_POINT('Ctrl Pts',(0.218997816432901,-0.0609635279872651,
-1.16365));
#30124=CARTESIAN_POINT('Ctrl Pts',(0.213991911411158,-0.0738045735508588,
-1.16365));
#30125=CARTESIAN_POINT('Ctrl Pts',(0.207900422173151,-0.086131422481015,
-1.16365));
#30126=CARTESIAN_POINT('Ctrl Pts',(0.202431471973834,-0.0971984900369931,
-1.16365));
#30127=CARTESIAN_POINT('Ctrl Pts',(0.196086562094324,-0.107851540751618,
-1.16365));
#30128=CARTESIAN_POINT('Ctrl Pts',(0.188909537892742,-0.117965068595534,
-1.16365));
#30129=CARTESIAN_POINT('Ctrl Pts',(0.186465674632955,-0.121408846745137,
-1.16365));
#30130=CARTESIAN_POINT('Ctrl Pts',(0.183929867562409,-0.124783110870494,
-1.16365));
#30131=CARTESIAN_POINT('Ctrl Pts',(0.181307798655181,-0.128079381800206,
-1.16365));
#30132=CARTESIAN_POINT('Ctrl Pts',(0.172609817251073,-0.139013840147387,
-1.16365));
#30133=CARTESIAN_POINT('Ctrl Pts',(0.162954416545594,-0.149107860965651,
-1.16365));
#30134=CARTESIAN_POINT('Ctrl Pts',(0.152416199398516,-0.158186984131325,
-1.16365));
#30135=CARTESIAN_POINT('Ctrl Pts',(0.144286167596249,-0.165191352995949,
-1.16365));
#30136=CARTESIAN_POINT('Ctrl Pts',(0.135629842554803,-0.17159127125675,
-1.16365));
#30137=CARTESIAN_POINT('Ctrl Pts',(0.126471106027295,-0.177287929553122,
-1.16365));
#30138=CARTESIAN_POINT('Origin',(0.,0.,-1.16365));
#30139=CARTESIAN_POINT('Origin',(0.,0.,-1.25608093797092));
#30140=CARTESIAN_POINT('Ctrl Pts',(0.126471106027295,-0.177287929553122,
-1.16365));
#30141=CARTESIAN_POINT('Ctrl Pts',(0.185290142270931,-0.135328453868889,
-1.16100984835807));
#30142=CARTESIAN_POINT('Ctrl Pts',(0.25689562471139,0.0109872606886212,
-1.15572954507421));
#30143=CARTESIAN_POINT('Ctrl Pts',(0.130348081000917,0.221923062878552,
-1.14780909014843));
#30144=CARTESIAN_POINT('Ctrl Pts',(-0.115118491958846,0.229917045457789,
-1.13988863522264));
#30145=CARTESIAN_POINT('Ctrl Pts',(-0.214016587705737,0.0882349264091937,
-1.13431258449681));
#30146=CARTESIAN_POINT('Ctrl Pts',(-0.218077155627143,0.00821599845413173,
-1.1313766854129));
#30147=CARTESIAN_POINT('Ctrl Pts',(-0.21801873929181,0.000148950382043584,
-1.13108093797092));
#30148=CARTESIAN_POINT('Ctrl Pts',(0.143065810904944,-0.200550483046316,
-1.18014778394209));
#30149=CARTESIAN_POINT('Ctrl Pts',(0.209602693369046,-0.153085361545635,
-1.17750763230016));
#30150=CARTESIAN_POINT('Ctrl Pts',(0.290603775215938,0.0124289366118328,
-1.17222732901631));
#30151=CARTESIAN_POINT('Ctrl Pts',(0.147451496978881,0.251042344346831,
-1.16430687409052));
#30152=CARTESIAN_POINT('Ctrl Pts',(-0.13022358165107,0.260085244626455,
-1.15638641916474));
#30153=CARTESIAN_POINT('Ctrl Pts',(-0.28913528563414,0.0324272013455538,
-1.14846596423895));
#30154=CARTESIAN_POINT('Ctrl Pts',(-0.184526815942454,-0.22498267491905,
-1.14054550931316));
#30155=CARTESIAN_POINT('Ctrl Pts',(0.0882987842694294,-0.277214481409077,
-1.13262505438738));
#30156=CARTESIAN_POINT('Ctrl Pts',(0.28062920438186,-0.0768131084218392,
-1.12470459946159));
#30157=CARTESIAN_POINT('Ctrl Pts',(0.217165088152307,0.193633152740157,
-1.11678414453581));
#30158=CARTESIAN_POINT('Ctrl Pts',(-0.0442519673101072,0.287563995963539,
-1.10886368961002));
#30159=CARTESIAN_POINT('Ctrl Pts',(-0.265331129903845,0.119382148576781,
-1.10094323468424));
#30160=CARTESIAN_POINT('Ctrl Pts',(-0.244556208400208,-0.157623085138064,
-1.09302277975845));
#30161=CARTESIAN_POINT('Ctrl Pts',(-0.000862913917304123,-0.290949477759334,
-1.08510232483266));
#30162=CARTESIAN_POINT('Ctrl Pts',(0.243616752571797,-0.15907058057088,
-1.07718186990688));
#30163=CARTESIAN_POINT('Ctrl Pts',(0.266034844651534,0.117805017487398,
-1.06926141498109));
#30164=CARTESIAN_POINT('Ctrl Pts',(0.0459566567534106,0.287298606742041,
-1.0613409600553));
#30165=CARTESIAN_POINT('Ctrl Pts',(-0.216011940049781,0.19491377884898,
-1.05342050512952));
#30166=CARTESIAN_POINT('Ctrl Pts',(-0.281081230017808,-0.0751390504041708,
-1.04550005020373));
#30167=CARTESIAN_POINT('Ctrl Pts',(-0.0899391959740744,-0.276701045494272,
-1.03757959527795));
#30168=CARTESIAN_POINT('Ctrl Pts',(0.183184259020086,-0.22604437666544,
-1.02965914035216));
#30169=CARTESIAN_POINT('Ctrl Pts',(0.289331500349707,0.0306563985282065,
-1.02173868542638));
#30170=CARTESIAN_POINT('Ctrl Pts',(0.131747133363499,0.259413229903282,
-1.01381823050059));
#30171=CARTESIAN_POINT('Ctrl Pts',(-0.145927451972247,0.25170957582738,
-1.0058977755748));
#30172=CARTESIAN_POINT('Ctrl Pts',(-0.290586166915714,0.014567469894556,
-0.997977320649018));
#30173=CARTESIAN_POINT('Ctrl Pts',(-0.170369620154127,-0.235853183175507,
-0.990056865723232));
#30174=CARTESIAN_POINT('Ctrl Pts',(0.105142335713471,-0.27128881444409,
-0.982136410797447));
#30175=CARTESIAN_POINT('Ctrl Pts',(0.284814892364508,-0.0594391171641165,
-0.97421595587166));
#30176=CARTESIAN_POINT('Ctrl Pts',(0.204872822781333,0.206590556507594,
-0.966295500945875));
#30177=CARTESIAN_POINT('Ctrl Pts',(-0.0618150340809172,0.284308693378328,
-0.958375046020089));
#30178=CARTESIAN_POINT('Ctrl Pts',(-0.272157217330499,0.102873614775734,
-0.950454591094303));
#30179=CARTESIAN_POINT('Ctrl Pts',(-0.234422505225032,-0.172332877320268,
-0.942534136168517));
#30180=CARTESIAN_POINT('Ctrl Pts',(0.0169931368468682,-0.290454410990472,
-0.934613681242732));
#30181=CARTESIAN_POINT('Ctrl Pts',(0.25291918554204,-0.143820781347327,
-0.926693226316945));
#30182=CARTESIAN_POINT('Ctrl Pts',(0.258304200125824,0.133908445439324,
-0.918772771391161));
#30183=CARTESIAN_POINT('Ctrl Pts',(0.0282396291651197,0.289577372920495,
-0.910852316465373));
#30184=CARTESIAN_POINT('Ctrl Pts',(-0.227565943992463,0.181290575313672,
-0.902931861539589));
#30185=CARTESIAN_POINT('Ctrl Pts',(-0.275940483620407,-0.0922463064956857,
-0.895011406613801));
#30186=CARTESIAN_POINT('Ctrl Pts',(-0.0727896029424237,-0.281698784637569,
-0.887090951688017));
#30187=CARTESIAN_POINT('Ctrl Pts',(0.196710496356156,-0.2143770327859,-0.87917049676223));
#30188=CARTESIAN_POINT('Ctrl Pts',(0.286904936603112,0.0483537890505052,
-0.871250041836445));
#30189=CARTESIAN_POINT('Ctrl Pts',(0.115579632374212,0.267009138688217,
-0.863329586910658));
#30190=CARTESIAN_POINT('Ctrl Pts',(-0.16109888146827,0.242280172429462,
-0.855409131984874));
#30191=CARTESIAN_POINT('Ctrl Pts',(-0.290932454907336,-0.00329214889838965,
-0.847488677059086));
#30192=CARTESIAN_POINT('Ctrl Pts',(-0.155575118186665,-0.245863608864721,
-0.839568222133302));
#30193=CARTESIAN_POINT('Ctrl Pts',(0.121592135214742,-0.264325337825753,
-0.831647767207515));
#30194=CARTESIAN_POINT('Ctrl Pts',(0.287925659130265,-0.0418490905179701,
-0.823727312281731));
#30195=CARTESIAN_POINT('Ctrl Pts',(0.191809029014613,0.218773462630297,
-0.815806857355942));
#30196=CARTESIAN_POINT('Ctrl Pts',(-0.0791454719650589,0.279979509661344,
-0.807886402430158));
#30197=CARTESIAN_POINT('Ctrl Pts',(-0.277957249122045,0.0859784811640934,
-0.799965947504372));
#30198=CARTESIAN_POINT('Ctrl Pts',(-0.223405282781762,-0.186393699432088,
-0.792045492578585));
#30199=CARTESIAN_POINT('Ctrl Pts',(0.0347851889093908,-0.288864193342333,
-0.784125037652801));
#30200=CARTESIAN_POINT('Ctrl Pts',(0.26126824621153,-0.128029040003937,
-0.776204582727013));
#30201=CARTESIAN_POINT('Ctrl Pts',(0.249599929062365,0.149507213788637,
-0.76828412780123));
#30202=CARTESIAN_POINT('Ctrl Pts',(0.0104161482811412,0.290764570430725,
-0.760363672875442));
#30203=CARTESIAN_POINT('Ctrl Pts',(-0.238262165669008,0.166984047062865,
-0.752443217949657));
#30204=CARTESIAN_POINT('Ctrl Pts',(-0.269759620266356,-0.109005866064766,
-0.744522763023871));
#30205=CARTESIAN_POINT('Ctrl Pts',(-0.0553656384972611,-0.285634692634787,
-0.736602308098084));
#30206=CARTESIAN_POINT('Ctrl Pts',(0.209495260307064,-0.201901628204565,
-0.7286818531723));
#30207=CARTESIAN_POINT('Ctrl Pts',(0.28339692504217,0.0658689186143308,
-0.720761398246513));
#30208=CARTESIAN_POINT('Ctrl Pts',(0.0989764699149806,0.273598592770407,
-0.712840943320728));
#30209=CARTESIAN_POINT('Ctrl Pts',(-0.17566307111485,0.231937528246891,
-0.704920488394942));
#30210=CARTESIAN_POINT('Ctrl Pts',(-0.290182113641896,-0.0211393586728707,
-0.697000033469155));
#30211=CARTESIAN_POINT('Ctrl Pts',(-0.140194197489197,-0.25494728583207,
-0.689079578543371));
#30212=CARTESIAN_POINT('Ctrl Pts',(0.137583610111387,-0.256365523796583,
-0.681159123617583));
#30213=CARTESIAN_POINT('Ctrl Pts',(0.289951130296208,-0.0241013195225775,
-0.673238668691798));
#30214=CARTESIAN_POINT('Ctrl Pts',(0.178022237866677,0.230131732683084,
-0.665318213766013));
#30215=CARTESIAN_POINT('Ctrl Pts',(-0.0961775820314826,0.274594982250872,
-0.657397758840226));
#30216=CARTESIAN_POINT('Ctrl Pts',(-0.282709559838887,0.0687592636557534,
-0.649477303914441));
#30217=CARTESIAN_POINT('Ctrl Pts',(-0.211545965289424,-0.199751936492601,
-0.641556848988655));
#30218=CARTESIAN_POINT('Ctrl Pts',(0.052446123054555,-0.286185142415403,
-0.633636394062869));
#30219=CARTESIAN_POINT('Ctrl Pts',(0.268632492673834,-0.111754711053366,
-0.625715939137084));
#30220=CARTESIAN_POINT('Ctrl Pts',(0.239954825885267,0.16454243555129,-0.617795484211296));
#30221=CARTESIAN_POINT('Ctrl Pts',(-0.00744659482069732,0.290855771454435,
-0.609875029285512));
#30222=CARTESIAN_POINT('Ctrl Pts',(-0.248060291349511,0.152048095740703,
-0.601954574359725));
#30223=CARTESIAN_POINT('Ctrl Pts',(-0.262561935655004,-0.125354543227901,
-0.594034119433939));
#30224=CARTESIAN_POINT('Ctrl Pts',(-0.0377329810012622,-0.288493940504021,
-0.586113664508154));
#30225=CARTESIAN_POINT('Ctrl Pts',(0.221490361098709,-0.18866518360085,
-0.578193209582367));
#30226=CARTESIAN_POINT('Ctrl Pts',(0.278820688305979,0.0831357644781028,
-0.570272754656583));
#30227=CARTESIAN_POINT('Ctrl Pts',(0.0820002294595659,0.279156755123992,
-0.562352299730795));
#30228=CARTESIAN_POINT('Ctrl Pts',(-0.189565123319758,0.220720627906736,
-0.554431844805011));
#30229=CARTESIAN_POINT('Ctrl Pts',(-0.288337971379312,-0.038906886583765,
-0.546511389879224));
#30230=CARTESIAN_POINT('Ctrl Pts',(-0.124284834321296,-0.263069974570467,
-0.538590934953439));
#30231=CARTESIAN_POINT('Ctrl Pts',(0.153056482782545,-0.247439375688298,
-0.530670480027653));
#30232=CARTESIAN_POINT('Ctrl Pts',(0.290883671124509,-0.00626270196536656,
-0.522750025101867));
#30233=CARTESIAN_POINT('Ctrl Pts',(0.163564416727095,0.240622553272764,
-0.514829570176081));
#30234=CARTESIAN_POINT('Ctrl Pts',(-0.112847164119155,0.268175407360637,
-0.506909115250295));
#30235=CARTESIAN_POINT('Ctrl Pts',(-0.286396236307729,0.0512808676949378,
-0.498988660324509));
#30236=CARTESIAN_POINT('Ctrl Pts',(-0.198889254791463,-0.212357236493779,
-0.491068205398723));
#30237=CARTESIAN_POINT('Ctrl Pts',(0.0699093688550693,-0.282427356516795,
-0.483147750472938));
#30238=CARTESIAN_POINT('Ctrl Pts',(0.274984166429074,-0.0950591383091926,
-0.475227295547151));
#30239=CARTESIAN_POINT('Ctrl Pts',(0.229405246465546,0.178957437556701,
-0.467306840621366));
#30240=CARTESIAN_POINT('Ctrl Pts',(-0.0252812690221513,0.289850632221853,
-0.459386385695579));
#30241=CARTESIAN_POINT('Ctrl Pts',(-0.256923388366033,0.136539020332266,
-0.451465930769795));
#30242=CARTESIAN_POINT('Ctrl Pts',(-0.254374560454433,-0.141230713927224,
-0.443545475844008));
#30243=CARTESIAN_POINT('Ctrl Pts',(-0.0199580942971045,-0.290265750709254,
-0.435625020918223));
#30244=CARTESIAN_POINT('Ctrl Pts',(0.232650584871963,-0.17471759190623,
-0.427704565992436));
#30245=CARTESIAN_POINT('Ctrl Pts',(0.273193475880536,0.100089241675063,
-0.419784111066651));
#30246=CARTESIAN_POINT('Ctrl Pts',(0.0647149005781834,0.283662675031338,
-0.411863656140865));
#30247=CARTESIAN_POINT('Ctrl Pts',(-0.202752636236533,0.208671751950079,
-0.403943201215079));
#30248=CARTESIAN_POINT('Ctrl Pts',(-0.285406979356585,-0.0565277604131661,
-0.396022746289293));
#30249=CARTESIAN_POINT('Ctrl Pts',(-0.107906996808085,-0.270201057737822,
-0.388102291363507));
#30250=CARTESIAN_POINT('Ctrl Pts',(0.16795243039314,-0.237580539371001,
-0.380181836437721));
#30251=CARTESIAN_POINT('Ctrl Pts',(0.290719766532602,0.0115995219732621,
-0.372261381511936));
#30252=CARTESIAN_POINT('Ctrl Pts',(0.148490062335797,0.250206380714582,
-0.364340926586149));
#30253=CARTESIAN_POINT('Ctrl Pts',(-0.129091384563791,0.260744982682662,
-0.356420471660364));
#30254=CARTESIAN_POINT('Ctrl Pts',(-0.28900338211591,0.033609175656999,
-0.348500016734578));
#30255=CARTESIAN_POINT('Ctrl Pts',(-0.185482858992497,-0.224162085515702,
-0.340579561808792));
#30256=CARTESIAN_POINT('Ctrl Pts',(0.0871091010420014,-0.27760500009624,
-0.332659106883006));
#30257=CARTESIAN_POINT('Ctrl Pts',(0.280299325729081,-0.0780052534038562,
-0.32473865195722));
#30258=CARTESIAN_POINT('Ctrl Pts',(0.217990955971174,0.192697884465696,
-0.316818197031434));
#30259=CARTESIAN_POINT('Ctrl Pts',(-0.0430206490067566,0.287752941465094,
-0.308897742105649));
#30260=CARTESIAN_POINT('Ctrl Pts',(-0.264818048510752,0.120515280133804,
-0.300977287179863));
#30261=CARTESIAN_POINT('Ctrl Pts',(-0.245228355833355,-0.156574535152013,
-0.293056832254077));
#30262=CARTESIAN_POINT('Ctrl Pts',(-0.00210797834057768,-0.290943444659053,
-0.285136377328291));
#30263=CARTESIAN_POINT('Ctrl Pts',(0.242933864720045,-0.160111426621978,
-0.277215922402505));
#30264=CARTESIAN_POINT('Ctrl Pts',(0.266536498758302,0.116665446438031,
-0.26929546747672));
#30265=CARTESIAN_POINT('Ctrl Pts',(0.0471856379063532,0.287099368055711,
-0.261375012550933));
#30266=CARTESIAN_POINT('Ctrl Pts',(-0.215175901374109,0.195836316934433,
-0.253454557625148));
#30267=CARTESIAN_POINT('Ctrl Pts',(-0.281400185540743,-0.0739355607360446,
-0.245534102699361));
#30268=CARTESIAN_POINT('Ctrl Pts',(-0.0911224189205789,-0.276313655709459,
-0.237613647773576));
#30269=CARTESIAN_POINT('Ctrl Pts',(0.182215304741336,-0.22682617635566,
-0.229693192847789));
#30270=CARTESIAN_POINT('Ctrl Pts',(0.289460034346049,0.0294180231372127,
-0.221772737922004));
#30271=CARTESIAN_POINT('Ctrl Pts',(0.132855995349668,0.258847090097914,
-0.213852282996218));
#30272=CARTESIAN_POINT('Ctrl Pts',(-0.144849013006134,0.252331716185271,
-0.205931828070432));
#30273=CARTESIAN_POINT('Ctrl Pts',(-0.29052117006007,0.0158107984837069,
-0.198011373144647));
#30274=CARTESIAN_POINT('Ctrl Pts',(-0.171377311300073,-0.23512198675802,
-0.19009091821886));
#30275=CARTESIAN_POINT('Ctrl Pts',(0.103980487374873,-0.271736250484141,
-0.182170463293075));
#30276=CARTESIAN_POINT('Ctrl Pts',(0.284557936296122,-0.0606573383293682,
-0.174250008367289));
#30277=CARTESIAN_POINT('Ctrl Pts',(0.205754978077643,0.205711983108962,
-0.166329553441503));
#30278=CARTESIAN_POINT('Ctrl Pts',(-0.0605978669457687,0.284570607032695,
-0.158409098515717));
#30279=CARTESIAN_POINT('Ctrl Pts',(-0.271714517213715,0.104037272696485,
-0.150488643589931));
#30280=CARTESIAN_POINT('Ctrl Pts',(-0.235157790958593,-0.17132816727427,
-0.142568188664145));
#30281=CARTESIAN_POINT('Ctrl Pts',(0.0157500716120863,-0.290524474026164,
-0.13464773373836));
#30282=CARTESIAN_POINT('Ctrl Pts',(0.252301461550156,-0.14490173197348,
-0.126727278812573));
#30283=CARTESIAN_POINT('Ctrl Pts',(0.258874807121329,0.132801874887983,
-0.118806823886788));
#30284=CARTESIAN_POINT('Ctrl Pts',(0.0294785960508995,0.289453922220514,
-0.110886368961002));
#30285=CARTESIAN_POINT('Ctrl Pts',(-0.226788243918246,0.182262624136886,
-0.102965914035216));
#30286=CARTESIAN_POINT('Ctrl Pts',(-0.276332402362021,-0.09106451907133,
-0.09504545910943));
#30287=CARTESIAN_POINT('Ctrl Pts',(-0.0739949199882418,-0.281385017105497,
-0.0871250041836446));
#30288=CARTESIAN_POINT('Ctrl Pts',(0.195792393150789,-0.215216274196785,
-0.0792045492578584));
#30289=CARTESIAN_POINT('Ctrl Pts',(0.287107229299654,0.0471245930402426,
-0.0712840943320728));
#30290=CARTESIAN_POINT('Ctrl Pts',(0.116724934327384,0.266514095421913,
-0.0633636394062869));
#30291=CARTESIAN_POINT('Ctrl Pts',(-0.160067851115533,0.242963550798627,
-0.0554431844805008));
#30292=CARTESIAN_POINT('Ctrl Pts',(-0.290930201862917,-0.00204001234416272,
-0.0475227295547152));
#30293=CARTESIAN_POINT('Ctrl Pts',(-0.156651773764553,-0.245209240429496,
-0.0396022746289292));
#30294=CARTESIAN_POINT('Ctrl Pts',(0.120509367727107,-0.264817350405622,
-0.0316818197031433));
#30295=CARTESIAN_POINT('Ctrl Pts',(0.287649633879381,-0.0431300802166473,
-0.0237613647773576));
#30296=CARTESIAN_POINT('Ctrl Pts',(0.192925896622358,0.218045410474343,
-0.0158409098515715));
#30297=CARTESIAN_POINT('Ctrl Pts',(-0.0783209863033229,0.280126499531071,
-0.00792045492578587));
#30298=CARTESIAN_POINT('Ctrl Pts',(-0.21054802840921,0.151782557364509,
-0.0026401516419286));
#30299=CARTESIAN_POINT('Ctrl Pts',(-0.235034375322676,0.0738049111962042,
0.));
#30300=CARTESIAN_POINT('Ctrl Pts',(0.137534242612394,-0.192796298548585,
-1.17464852262806));
#30301=CARTESIAN_POINT('Ctrl Pts',(0.201498509669674,-0.147166392320053,
-1.17200837098613));
#30302=CARTESIAN_POINT('Ctrl Pts',(0.279367725047756,0.0119483779707621,
-1.16672806770228));
#30303=CARTESIAN_POINT('Ctrl Pts',(0.14175035831956,0.241335917190738,-1.15880761277649));
#30304=CARTESIAN_POINT('Ctrl Pts',(-0.125188551753662,0.250029178236899,
-1.15088715785071));
#30305=CARTESIAN_POINT('Ctrl Pts',(-0.277956013883926,0.0311734197631856,
-1.14296670292492));
#30306=CARTESIAN_POINT('Ctrl Pts',(-0.177392178549103,-0.216283831896505,
-1.13504624799913));
#30307=CARTESIAN_POINT('Ctrl Pts',(0.0848847557727121,-0.266496121614389,
-1.12712579307335));
#30308=CARTESIAN_POINT('Ctrl Pts',(0.269778816024899,-0.0738431678587459,
-1.11920533814756));
#30309=CARTESIAN_POINT('Ctrl Pts',(0.208768508226792,0.186146423371982,
-1.11128488322178));
#30310=CARTESIAN_POINT('Ctrl Pts',(-0.0425409870437026,0.276445477345505,
-1.10336442829599));
#30311=CARTESIAN_POINT('Ctrl Pts',(-0.255072233973931,0.114766297287177,
-1.09544397337021));
#30312=CARTESIAN_POINT('Ctrl Pts',(-0.235100564458613,-0.151528667090814,
-1.08752351844442));
#30313=CARTESIAN_POINT('Ctrl Pts',(-0.000829549780659682,-0.279700061174566,
-1.07960306351863));
#30314=CARTESIAN_POINT('Ctrl Pts',(0.2341974322217,-0.152920195833971,-1.07168260859285));
#30315=CARTESIAN_POINT('Ctrl Pts',(0.255748739941544,0.11325014518552,-1.06376215366706));
#30316=CARTESIAN_POINT('Ctrl Pts',(0.0441797655190845,0.27619034926602,
-1.05584169874127));
#30317=CARTESIAN_POINT('Ctrl Pts',(-0.207659946021065,0.187377534710411,
-1.04792124381549));
#30318=CARTESIAN_POINT('Ctrl Pts',(-0.270213364314866,-0.0722338364601898,
-1.0400007888897));
#30319=CARTESIAN_POINT('Ctrl Pts',(-0.0864617417761726,-0.266002537443397,
-1.03208033396392));
#30320=CARTESIAN_POINT('Ctrl Pts',(0.176101530921177,-0.217304483473891,
-1.02415987903813));
#30321=CARTESIAN_POINT('Ctrl Pts',(0.278144642055285,0.0294710841544246,
-1.01623942411235));
#30322=CARTESIAN_POINT('Ctrl Pts',(0.126653196098277,0.24938314662815,-1.00831896918656));
#30323=CARTESIAN_POINT('Ctrl Pts',(-0.140285239753713,0.241977350498556,
-1.00039851426077));
#30324=CARTESIAN_POINT('Ctrl Pts',(-0.279350797563686,0.0140042259296867,
-0.992478059334987));
#30325=CARTESIAN_POINT('Ctrl Pts',(-0.163782363681758,-0.226734037367727,
-0.984557604409201));
#30326=CARTESIAN_POINT('Ctrl Pts',(0.101077059692887,-0.260799567609992,
-0.976637149483415));
#30327=CARTESIAN_POINT('Ctrl Pts',(0.273802666467321,-0.0571409333159812,
-0.968716694557631));
#30328=CARTESIAN_POINT('Ctrl Pts',(0.19695151717146,0.198602835579099,-0.960796239631843));
#30329=CARTESIAN_POINT('Ctrl Pts',(-0.059424986589053,0.273316039412716,
-0.952875784706058));
#30330=CARTESIAN_POINT('Ctrl Pts',(-0.261634394131502,0.0988960577197611,
-0.944955329780273));
#30331=CARTESIAN_POINT('Ctrl Pts',(-0.225358675867337,-0.165669712487812,
-0.937034874854486));
#30332=CARTESIAN_POINT('Ctrl Pts',(0.0163361056779362,-0.279224135915642,
-0.9291144199287));
#30333=CARTESIAN_POINT('Ctrl Pts',(0.243140191256317,-0.138260022498806,
-0.921193965002915));
#30334=CARTESIAN_POINT('Ctrl Pts',(0.248316996934436,0.128730942119617,
-0.913273510077128));
#30335=CARTESIAN_POINT('Ctrl Pts',(0.027147757974546,0.278381008085635,
-0.905353055151344));
#30336=CARTESIAN_POINT('Ctrl Pts',(-0.218767220158372,0.174281065551697,
-0.897432600225556));
#30337=CARTESIAN_POINT('Ctrl Pts',(-0.265271382315417,-0.0886796490190409,
-0.889512145299772));
#30338=CARTESIAN_POINT('Ctrl Pts',(-0.0699752292138806,-0.270807041492966,
-0.881591690373984));
#30339=CARTESIAN_POINT('Ctrl Pts',(0.189104783030431,-0.206088251631909,
-0.8736712354482));
#30340=CARTESIAN_POINT('Ctrl Pts',(0.275811900186857,0.0464842138903423,
-0.865750780522412));
#30341=CARTESIAN_POINT('Ctrl Pts',(0.111110803478883,0.256685363384765,
-0.857830325596628));
#30342=CARTESIAN_POINT('Ctrl Pts',(-0.154870073487814,0.232912530284584,
-0.849909870670842));
#30343=CARTESIAN_POINT('Ctrl Pts',(-0.279683696502658,-0.00316485960162851,
-0.841989415745056));
#30344=CARTESIAN_POINT('Ctrl Pts',(-0.14955988376114,-0.23635741493561,
-0.834068960819269));
#30345=CARTESIAN_POINT('Ctrl Pts',(0.116890835892962,-0.254105330345378,
-0.826148505893485));
#30346=CARTESIAN_POINT('Ctrl Pts',(0.276793156986097,-0.0402310162854403,
-0.818228050967698));
#30347=CARTESIAN_POINT('Ctrl Pts',(0.184392828481371,0.210314695707002,
-0.810307596041912));
#30348=CARTESIAN_POINT('Ctrl Pts',(-0.0760853517277248,0.269154241427026,
-0.802387141116127));
#30349=CARTESIAN_POINT('Ctrl Pts',(-0.267210170583837,0.0826541660307953,
-0.794466686190341));
#30350=CARTESIAN_POINT('Ctrl Pts',(-0.21476742884023,-0.179186879918832,
-0.786546231264554));
#30351=CARTESIAN_POINT('Ctrl Pts',(0.0334402369127925,-0.277695403240503,
-0.77862577633877));
#30352=CARTESIAN_POINT('Ctrl Pts',(0.251166439655148,-0.123078860965831,
-0.770705321412982));
#30353=CARTESIAN_POINT('Ctrl Pts',(0.239949272174526,0.143726591863178,
-0.762784866487197));
#30354=CARTESIAN_POINT('Ctrl Pts',(0.010013413097955,0.279522303195683,
-0.754864411561412));
#30355=CARTESIAN_POINT('Ctrl Pts',(-0.229049877753451,0.160527692087124,
-0.746943956635625));
#30356=CARTESIAN_POINT('Ctrl Pts',(-0.259329498963182,-0.10479120856825,
-0.73902350170984));
#30357=CARTESIAN_POINT('Ctrl Pts',(-0.0532249536720674,-0.274590769568636,
-0.731103046784054));
#30358=CARTESIAN_POINT('Ctrl Pts',(0.201395230453503,-0.194095202352532,
-0.723182591858267));
#30359=CARTESIAN_POINT('Ctrl Pts',(0.272439524144964,0.0633221296969308,
-0.715262136932483));
#30360=CARTESIAN_POINT('Ctrl Pts',(0.0951495940231997,0.263020039508227,
-0.707341682006696));
#30361=CARTESIAN_POINT('Ctrl Pts',(-0.168871145998678,0.222969779285854,
-0.69942122708091));
#30362=CARTESIAN_POINT('Ctrl Pts',(-0.278962366808371,-0.0203220159029941,
-0.691500772155125));
#30363=CARTESIAN_POINT('Ctrl Pts',(-0.134773658698514,-0.245089876059184,
-0.683580317229338));
#30364=CARTESIAN_POINT('Ctrl Pts',(0.132264008380877,-0.246453278559472,
-0.675659862303554));
#30365=CARTESIAN_POINT('Ctrl Pts',(0.278740314318651,-0.0231694540123176,
-0.667739407377766));
#30366=CARTESIAN_POINT('Ctrl Pts',(0.171139096743559,0.221233803907739,
-0.659818952451982));
#30367=CARTESIAN_POINT('Ctrl Pts',(-0.0924589237451018,0.263977904085905,
-0.651898497526195));
#30368=CARTESIAN_POINT('Ctrl Pts',(-0.27177873557477,0.0661007209875132,
-0.643978042600409));
#30369=CARTESIAN_POINT('Ctrl Pts',(-0.203366645949535,-0.192028627399474,
-0.636057587674623));
#30370=CARTESIAN_POINT('Ctrl Pts',(0.0504183198392325,-0.27511993648276,
-0.628137132748838));
#30371=CARTESIAN_POINT('Ctrl Pts',(0.258245951197406,-0.107433770835046,
-0.620216677823051));
#30372=CARTESIAN_POINT('Ctrl Pts',(0.230677092105858,0.158180484268051,
-0.612296222897266));
#30373=CARTESIAN_POINT('Ctrl Pts',(-0.00715867594240549,0.279609977977254,
-0.604375767971481));
#30374=CARTESIAN_POINT('Ctrl Pts',(-0.238469163786677,0.146169231880625,
-0.596455313045694));
#30375=CARTESIAN_POINT('Ctrl Pts',(-0.252410109240903,-0.120507772275005,
-0.588534858119908));
#30376=CARTESIAN_POINT('Ctrl Pts',(-0.0362740540922425,-0.277339466043697,
-0.580614403194122));
#30377=CARTESIAN_POINT('Ctrl Pts',(0.212926546649896,-0.181370538284032,
-0.572693948268336));
#30378=CARTESIAN_POINT('Ctrl Pts',(0.268040225321954,0.0799213615690144,
-0.564773493342551));
#30379=CARTESIAN_POINT('Ctrl Pts',(0.0788297314461609,0.268363298283903,
-0.556853038416765));
#30380=CARTESIAN_POINT('Ctrl Pts',(-0.182235682282126,0.212186574808252,
-0.548932583490979));
#30381=CARTESIAN_POINT('Ctrl Pts',(-0.277189527387479,-0.0374025712003252,
-0.541012128565193));
#30382=CARTESIAN_POINT('Ctrl Pts',(-0.119479423130266,-0.252898505084842,
-0.533091673639407));
#30383=CARTESIAN_POINT('Ctrl Pts',(0.147138630139948,-0.237872255520119,
-0.525171218713621));
#30384=CARTESIAN_POINT('Ctrl Pts',(0.279636798920486,-0.00602055771442263,
-0.517250763787836));
#30385=CARTESIAN_POINT('Ctrl Pts',(0.157240280054371,0.23131900214663,-0.509330308862049));
#30386=CARTESIAN_POINT('Ctrl Pts',(-0.108483984747388,0.257806538860088,
-0.501409853936264));
#30387=CARTESIAN_POINT('Ctrl Pts',(-0.275322868534921,0.0492981184974779,
-0.493489399010478));
#30388=CARTESIAN_POINT('Ctrl Pts',(-0.191199300856458,-0.204146549757009,
-0.485568944084692));
#30389=CARTESIAN_POINT('Ctrl Pts',(0.0672063579423657,-0.271507443503511,
-0.477648489158906));
#30390=CARTESIAN_POINT('Ctrl Pts',(0.264352040651778,-0.0913837240920417,
-0.46972803423312));
#30391=CARTESIAN_POINT('Ctrl Pts',(0.220535406917812,0.172038137403554,
-0.461807579307335));
#30392=CARTESIAN_POINT('Ctrl Pts',(-0.0243037813524294,0.278643701952265,
-0.453887124381548));
#30393=CARTESIAN_POINT('Ctrl Pts',(-0.246989573573313,0.131259807145073,
-0.445966669455763));
#30394=CARTESIAN_POINT('Ctrl Pts',(-0.244539294822899,-0.135770098744935,
-0.438046214529977));
#30395=CARTESIAN_POINT('Ctrl Pts',(-0.0191864245257226,-0.279042770090194,
-0.430125759604191));
#30396=CARTESIAN_POINT('Ctrl Pts',(0.223655265931815,-0.16796222327255,
-0.422205304678406));
#30397=CARTESIAN_POINT('Ctrl Pts',(0.262630586261044,0.0962193410176438,
-0.414284849752619));
#30398=CARTESIAN_POINT('Ctrl Pts',(0.0622127311931329,0.272694999043218,
-0.406364394826833));
#30399=CARTESIAN_POINT('Ctrl Pts',(-0.194913306582979,0.200603562636807,
-0.398443939901048));
#30400=CARTESIAN_POINT('Ctrl Pts',(-0.274371860710872,-0.0543421427231499,
-0.390523484975262));
#30401=CARTESIAN_POINT('Ctrl Pts',(-0.103734826543839,-0.259753868474771,
-0.382603030049476));
#30402=CARTESIAN_POINT('Ctrl Pts',(0.161458633358455,-0.228394606196619,
-0.37468257512369));
#30403=CARTESIAN_POINT('Ctrl Pts',(0.279479231617956,0.0111510322359151,
-0.366762120197904));
#30404=CARTESIAN_POINT('Ctrl Pts',(0.142748768064441,0.24053227567579,-0.358841665272119));
#30405=CARTESIAN_POINT('Ctrl Pts',(-0.124100130502618,0.250663407849894,
-0.350921210346332));
#30406=CARTESIAN_POINT('Ctrl Pts',(-0.277829210349505,0.0323096936268268,
-0.343000755420547));
#30407=CARTESIAN_POINT('Ctrl Pts',(-0.178311256670989,-0.215494970173559,
-0.33508030049476));
#30408=CARTESIAN_POINT('Ctrl Pts',(0.0837410710544831,-0.266871541091098,
-0.327159845568975));
#30409=CARTESIAN_POINT('Ctrl Pts',(0.26946169196586,-0.074989219149049,
-0.319239390643189));
#30410=CARTESIAN_POINT('Ctrl Pts',(0.209562444277951,0.185247316779332,
-0.311318935717403));
#30411=CARTESIAN_POINT('Ctrl Pts',(-0.0413572770490159,0.276627117363389,
-0.303398480791617));
#30412=CARTESIAN_POINT('Ctrl Pts',(-0.254578990617248,0.115855616877159,
-0.295478025865831));
#30413=CARTESIAN_POINT('Ctrl Pts',(-0.235746723646171,-0.150520658767508,
-0.287557570940046));
#30414=CARTESIAN_POINT('Ctrl Pts',(-0.00202647440839203,-0.279694261341101,
-0.27963711601426));
#30415=CARTESIAN_POINT('Ctrl Pts',(0.233540947888471,-0.15392079809113,
-0.271716661088474));
#30416=CARTESIAN_POINT('Ctrl Pts',(0.256230997842236,0.112154635082958,
-0.263796206162688));
#30417=CARTESIAN_POINT('Ctrl Pts',(0.045361228728119,0.275998814044221,
-0.255875751236902));
#30418=CARTESIAN_POINT('Ctrl Pts',(-0.206856232364211,0.188264403320467,
-0.247955296311116));
#30419=CARTESIAN_POINT('Ctrl Pts',(-0.270519987581435,-0.0710768791204128,
-0.240034841385331));
#30420=CARTESIAN_POINT('Ctrl Pts',(-0.087599215997021,-0.265630125891588,
-0.232114386459544));
#30421=CARTESIAN_POINT('Ctrl Pts',(0.175170040776809,-0.218056055268639,
-0.224193931533759));
#30422=CARTESIAN_POINT('Ctrl Pts',(0.278268206348704,0.0282805899308719,
-0.216273476607973));
#30423=CARTESIAN_POINT('Ctrl Pts',(0.127719184488269,0.248838896336264,
-0.208353021682187));
#30424=CARTESIAN_POINT('Ctrl Pts',(-0.139248498092866,0.242575436109506,
-0.200432566756401));
#30425=CARTESIAN_POINT('Ctrl Pts',(-0.279288313779079,0.0151994818384572,
-0.192512111830616));
#30426=CARTESIAN_POINT('Ctrl Pts',(-0.164751092951653,-0.226031112295385,
-0.184591656904829));
#30427=CARTESIAN_POINT('Ctrl Pts',(0.099960133641381,-0.261229703758501,
-0.176671201979044));
#30428=CARTESIAN_POINT('Ctrl Pts',(0.273555645477285,-0.0583120525668871,
-0.168750747053258));
#30429=CARTESIAN_POINT('Ctrl Pts',(0.197799564372794,0.197758231783153,
-0.160830292127472));
#30430=CARTESIAN_POINT('Ctrl Pts',(-0.0582548806147009,0.273567826306141,
-0.152909837201686));
#30431=CARTESIAN_POINT('Ctrl Pts',(-0.261208810794147,0.100014723386828,
-0.1449893822759));
#30432=CARTESIAN_POINT('Ctrl Pts',(-0.226065532144383,-0.164703849055121,
-0.137068927350114));
#30433=CARTESIAN_POINT('Ctrl Pts',(0.0151411029410687,-0.27929148999897,
-0.129148472424328));
#30434=CARTESIAN_POINT('Ctrl Pts',(0.242546351254783,-0.139299178707609,
-0.121228017498542));
#30435=CARTESIAN_POINT('Ctrl Pts',(0.248865541694779,0.127667156567268,
-0.113307562572757));
#30436=CARTESIAN_POINT('Ctrl Pts',(0.0283388208230337,0.278262330545457,
-0.105387107646971));
#30437=CARTESIAN_POINT('Ctrl Pts',(-0.218019589470017,0.175215530591508,
-0.097466652721185));
#30438=CARTESIAN_POINT('Ctrl Pts',(-0.265648147714169,-0.0875435548165934,
-0.0895461977953989));
#30439=CARTESIAN_POINT('Ctrl Pts',(-0.0711339432767014,-0.270505405626179,
-0.0816257428696132));
#30440=CARTESIAN_POINT('Ctrl Pts',(0.188222177828032,-0.206895044191815,
-0.0737052879438272));
#30441=CARTESIAN_POINT('Ctrl Pts',(0.276006371337084,0.0453025441313394,
-0.0657848330180416));
#30442=CARTESIAN_POINT('Ctrl Pts',(0.112211822902711,0.256209460719685,
-0.0578643780922556));
#30443=CARTESIAN_POINT('Ctrl Pts',(-0.153878907409929,0.233569486169616,
-0.0499439231664696));
#30444=CARTESIAN_POINT('Ctrl Pts',(-0.279681530571079,-0.00196113628336259,
-0.042023468240684));
#30445=CARTESIAN_POINT('Ctrl Pts',(-0.15059491098758,-0.235728347329877,
-0.0341030133148979));
#30446=CARTESIAN_POINT('Ctrl Pts',(0.115849933070721,-0.254578319504005,
-0.0261825583891122));
#30447=CARTESIAN_POINT('Ctrl Pts',(0.276527804114002,-0.0414624771557032,
-0.0182621034633263));
#30448=CARTESIAN_POINT('Ctrl Pts',(0.18546651295957,0.209614793324889,-0.0103416485375403));
#30449=CARTESIAN_POINT('Ctrl Pts',(-0.0752927443932796,0.269295548006681,
-0.00242119361175462));
#30450=CARTESIAN_POINT('Ctrl Pts',(-0.202407293801547,0.145913960413436,
0.00285910967210262));
#30451=CARTESIAN_POINT('Ctrl Pts',(-0.225946888312534,0.0709512810799313,
0.00549926131403122));
#30452=CARTESIAN_POINT('Ctrl Pts',(0.132002674319845,-0.185042114050853,
-1.16914926131403));
#30453=CARTESIAN_POINT('Ctrl Pts',(0.193394325970303,-0.141247423094471,
-1.1665091096721));
#30454=CARTESIAN_POINT('Ctrl Pts',(0.268131674879573,0.0114678193296916,
-1.16122880638824));
#30455=CARTESIAN_POINT('Ctrl Pts',(0.136049219660238,0.231629490034645,
-1.15330835146246));
#30456=CARTESIAN_POINT('Ctrl Pts',(-0.120153521856254,0.239973111847344,
-1.14538789653667));
#30457=CARTESIAN_POINT('Ctrl Pts',(-0.266776742133712,0.0299196381808178,
-1.13746744161089));
#30458=CARTESIAN_POINT('Ctrl Pts',(-0.170257541155753,-0.207584988873961,
-1.1295469866851));
#30459=CARTESIAN_POINT('Ctrl Pts',(0.0814707272759947,-0.2557777618197,
-1.12162653175932));
#30460=CARTESIAN_POINT('Ctrl Pts',(0.258928427667939,-0.070873227295653,
-1.11370607683353));
#30461=CARTESIAN_POINT('Ctrl Pts',(0.200371928301276,0.178659694003806,
-1.10578562190774));
#30462=CARTESIAN_POINT('Ctrl Pts',(-0.0408300067772977,0.265326958727471,
-1.09786516698196));
#30463=CARTESIAN_POINT('Ctrl Pts',(-0.244813338044019,0.110150445997574,
-1.08994471205617));
#30464=CARTESIAN_POINT('Ctrl Pts',(-0.225644920517017,-0.145434249043564,
-1.08202425713039));
#30465=CARTESIAN_POINT('Ctrl Pts',(-0.000796185644015697,-0.268450644589798,
-1.0741038022046));
#30466=CARTESIAN_POINT('Ctrl Pts',(0.224778111871604,-0.146769811097062,
-1.06618334727881));
#30467=CARTESIAN_POINT('Ctrl Pts',(0.245462635231555,0.108695272883643,
-1.05826289235303));
#30468=CARTESIAN_POINT('Ctrl Pts',(0.0424028742847586,0.265082091789998,
-1.05034243742724));
#30469=CARTESIAN_POINT('Ctrl Pts',(-0.199307951992349,0.179841290571841,
-1.04242198250146));
#30470=CARTESIAN_POINT('Ctrl Pts',(-0.259345498611925,-0.0693286225162085,
-1.03450152757567));
#30471=CARTESIAN_POINT('Ctrl Pts',(-0.0829842875782713,-0.255304029392523,
-1.02658107264989));
#30472=CARTESIAN_POINT('Ctrl Pts',(0.169018802822267,-0.208564590282341,
-1.0186606177241));
#30473=CARTESIAN_POINT('Ctrl Pts',(0.266957783760862,0.0282857697806424,
-1.01074016279831));
#30474=CARTESIAN_POINT('Ctrl Pts',(0.121559258833056,0.239353063353018,
-1.00281970787253));
#30475=CARTESIAN_POINT('Ctrl Pts',(-0.13464302753518,0.232245125169732,
-0.994899252946743));
#30476=CARTESIAN_POINT('Ctrl Pts',(-0.268115428211658,0.0134409819648169,
-0.986978798020956));
#30477=CARTESIAN_POINT('Ctrl Pts',(-0.157195107209389,-0.217614891559946,
-0.97905834309517));
#30478=CARTESIAN_POINT('Ctrl Pts',(0.0970117836723027,-0.250310320775895,
-0.971137888169384));
#30479=CARTESIAN_POINT('Ctrl Pts',(0.262790440570134,-0.0548427494678456,
-0.963217433243599));
#30480=CARTESIAN_POINT('Ctrl Pts',(0.189030211561587,0.190615114650604,
-0.955296978317811));
#30481=CARTESIAN_POINT('Ctrl Pts',(-0.0570349390971887,0.262323385447104,
-0.947376523392028));
#30482=CARTESIAN_POINT('Ctrl Pts',(-0.251111570932505,0.0949185006637886,
-0.93945606846624));
#30483=CARTESIAN_POINT('Ctrl Pts',(-0.21629484650964,-0.159006547655356,
-0.931535613540455));
#30484=CARTESIAN_POINT('Ctrl Pts',(0.0156790745090038,-0.267993860840813,
-0.923615158614669));
#30485=CARTESIAN_POINT('Ctrl Pts',(0.233361196970594,-0.132699263650284,
-0.915694703688884));
#30486=CARTESIAN_POINT('Ctrl Pts',(0.238329793743047,0.123553438799912,
-0.907774248763097));
#30487=CARTESIAN_POINT('Ctrl Pts',(0.026055886783973,0.267184643250775,
-0.899853793837312));
#30488=CARTESIAN_POINT('Ctrl Pts',(-0.209968496324281,0.167271555789721,
-0.891933338911526));
#30489=CARTESIAN_POINT('Ctrl Pts',(-0.254602281010427,-0.0851129915423963,
-0.884012883985739));
#30490=CARTESIAN_POINT('Ctrl Pts',(-0.0671608554853375,-0.259915298348364,
-0.876092429059954));
#30491=CARTESIAN_POINT('Ctrl Pts',(0.181499069704705,-0.197799470477918,
-0.868171974134168));
#30492=CARTESIAN_POINT('Ctrl Pts',(0.264718863770601,0.0446146387301797,
-0.860251519208382));
#30493=CARTESIAN_POINT('Ctrl Pts',(0.106641974583553,0.246361588081314,
-0.852331064282595));
#30494=CARTESIAN_POINT('Ctrl Pts',(-0.148641265507358,0.223544888139707,
-0.844410609356812));
#30495=CARTESIAN_POINT('Ctrl Pts',(-0.268434938097981,-0.00303757030486697,
-0.836490154431023));
#30496=CARTESIAN_POINT('Ctrl Pts',(-0.143544649335616,-0.226851221006499,
-0.828569699505241));
#30497=CARTESIAN_POINT('Ctrl Pts',(0.112189536571183,-0.243885322865004,
-0.82064924457945));
#30498=CARTESIAN_POINT('Ctrl Pts',(0.265660654841929,-0.0386129420529108,
-0.812728789653669));
#30499=CARTESIAN_POINT('Ctrl Pts',(0.176976627948129,0.201855928783708,
-0.804808334727879));
#30500=CARTESIAN_POINT('Ctrl Pts',(-0.0730252314903912,0.258328973192708,
-0.796887879802097));
#30501=CARTESIAN_POINT('Ctrl Pts',(-0.256463092045629,0.0793298508974973,
-0.788967424876308));
#30502=CARTESIAN_POINT('Ctrl Pts',(-0.206129574898699,-0.171980060405576,
-0.781046969950524));
#30503=CARTESIAN_POINT('Ctrl Pts',(0.0320952849161942,-0.266526613138673,
-0.773126515024738));
#30504=CARTESIAN_POINT('Ctrl Pts',(0.241064633098765,-0.118128681927724,
-0.765206060098951));
#30505=CARTESIAN_POINT('Ctrl Pts',(0.230298615286688,0.137945969937719,
-0.757285605173167));
#30506=CARTESIAN_POINT('Ctrl Pts',(0.00961067791476936,0.26828003596064,
-0.749365150247379));
#30507=CARTESIAN_POINT('Ctrl Pts',(-0.219837589837895,0.154071337111383,
-0.741444695321596));
#30508=CARTESIAN_POINT('Ctrl Pts',(-0.248899377660007,-0.100576551071733,
-0.733524240395808));
#30509=CARTESIAN_POINT('Ctrl Pts',(-0.051084268846874,-0.263546846502485,
-0.725603785470023));
#30510=CARTESIAN_POINT('Ctrl Pts',(0.193295200599941,-0.186288776500498,
-0.717683330544237));
#30511=CARTESIAN_POINT('Ctrl Pts',(0.261482123247759,0.0607753407795304,
-0.709762875618451));
#30512=CARTESIAN_POINT('Ctrl Pts',(0.0913227181314191,0.252441486246047,
-0.701842420692664));
#30513=CARTESIAN_POINT('Ctrl Pts',(-0.162079220882506,0.214002030324816,
-0.69392196576688));
#30514=CARTESIAN_POINT('Ctrl Pts',(-0.267742619974845,-0.0195046731331173,
-0.686001510841093));
#30515=CARTESIAN_POINT('Ctrl Pts',(-0.129353119907832,-0.235232466286298,
-0.678081055915308));
#30516=CARTESIAN_POINT('Ctrl Pts',(0.126944406650368,-0.23654103332236,
-0.670160600989521));
#30517=CARTESIAN_POINT('Ctrl Pts',(0.267529498341093,-0.0222375885020577,
-0.662240146063737));
#30518=CARTESIAN_POINT('Ctrl Pts',(0.164255955620441,0.212335875132393,
-0.654319691137949));
#30519=CARTESIAN_POINT('Ctrl Pts',(-0.0887402654587212,0.253360825920938,
-0.646399236212163));
#30520=CARTESIAN_POINT('Ctrl Pts',(-0.260847911310652,0.0634421783192726,
-0.638478781286379));
#30521=CARTESIAN_POINT('Ctrl Pts',(-0.195187326609645,-0.184305318306346,
-0.630558326360592));
#30522=CARTESIAN_POINT('Ctrl Pts',(0.0483905166239101,-0.264054730550116,
-0.622637871434807));
#30523=CARTESIAN_POINT('Ctrl Pts',(0.247859409720977,-0.103112830616725,
-0.614717416509021));
#30524=CARTESIAN_POINT('Ctrl Pts',(0.221399358326451,0.151818532984811,
-0.606796961583234));
#30525=CARTESIAN_POINT('Ctrl Pts',(-0.00687075706411388,0.268364184500074,
-0.598876506657451));
#30526=CARTESIAN_POINT('Ctrl Pts',(-0.228878036223844,0.140290368020547,
-0.590956051731662));
#30527=CARTESIAN_POINT('Ctrl Pts',(-0.242258282826801,-0.11566100132211,
-0.583035596805878));
#30528=CARTESIAN_POINT('Ctrl Pts',(-0.0348151271832227,-0.266184991583373,
-0.575115141880091));
#30529=CARTESIAN_POINT('Ctrl Pts',(0.204362732201082,-0.174075892967214,
-0.567194686954306));
#30530=CARTESIAN_POINT('Ctrl Pts',(0.25725976233793,0.0767069586599257,
-0.55927423202852));
#30531=CARTESIAN_POINT('Ctrl Pts',(0.0756592334327556,0.257569841443814,
-0.551353777102734));
#30532=CARTESIAN_POINT('Ctrl Pts',(-0.174906241244494,0.203652521709767,
-0.543433322176948));
#30533=CARTESIAN_POINT('Ctrl Pts',(-0.266041083395647,-0.0358982558168854,
-0.535512867251162));
#30534=CARTESIAN_POINT('Ctrl Pts',(-0.114674011939236,-0.242727035599217,
-0.527592412325376));
#30535=CARTESIAN_POINT('Ctrl Pts',(0.141220777497351,-0.228305135351939,
-0.519671957399591));
#30536=CARTESIAN_POINT('Ctrl Pts',(0.268389926716464,-0.0057784134634781,
-0.511751502473804));
#30537=CARTESIAN_POINT('Ctrl Pts',(0.150916143381647,0.222015451020496,
-0.503831047548019));
#30538=CARTESIAN_POINT('Ctrl Pts',(-0.10412080537562,0.24743767035954,-0.495910592622232));
#30539=CARTESIAN_POINT('Ctrl Pts',(-0.264249500762114,0.0473153693000177,
-0.487990137696447));
#30540=CARTESIAN_POINT('Ctrl Pts',(-0.183509346921452,-0.195935863020239,
-0.480069682770661));
#30541=CARTESIAN_POINT('Ctrl Pts',(0.064503347029662,-0.260587530490228,
-0.472149227844876));
#30542=CARTESIAN_POINT('Ctrl Pts',(0.253719914874482,-0.0877083098748911,
-0.464228772919089));
#30543=CARTESIAN_POINT('Ctrl Pts',(0.211665567370078,0.165118837250408,
-0.456308317993303));
#30544=CARTESIAN_POINT('Ctrl Pts',(-0.0233262936827075,0.267436771682676,
-0.448387863067517));
#30545=CARTESIAN_POINT('Ctrl Pts',(-0.237055758780593,0.125980593957881,
-0.440467408141732));
#30546=CARTESIAN_POINT('Ctrl Pts',(-0.234704029191364,-0.130309483562646,
-0.432546953215946));
#30547=CARTESIAN_POINT('Ctrl Pts',(-0.0184147547543408,-0.267819789471133,
-0.42462649829016));
#30548=CARTESIAN_POINT('Ctrl Pts',(0.214659946991667,-0.161206854638871,
-0.416706043364374));
#30549=CARTESIAN_POINT('Ctrl Pts',(0.25206769664155,0.0923494403602257,
-0.408785588438588));
#30550=CARTESIAN_POINT('Ctrl Pts',(0.0597105618080826,0.261727323055098,
-0.400865133512803));
#30551=CARTESIAN_POINT('Ctrl Pts',(-0.187073976929425,0.192535373323535,
-0.392944678587016));
#30552=CARTESIAN_POINT('Ctrl Pts',(-0.263336742065158,-0.0521565250331341,
-0.385024223661231));
#30553=CARTESIAN_POINT('Ctrl Pts',(-0.0995626562795935,-0.249306679211719,
-0.377103768735445));
#30554=CARTESIAN_POINT('Ctrl Pts',(0.15496483632377,-0.219208673022239,
-0.369183313809659));
#30555=CARTESIAN_POINT('Ctrl Pts',(0.26823869670331,0.0107025424985688,
-0.361262858883874));
#30556=CARTESIAN_POINT('Ctrl Pts',(0.137007473793086,0.230858170636998,
-0.353342403958087));
#30557=CARTESIAN_POINT('Ctrl Pts',(-0.119108876441444,0.240581833017126,
-0.345421949032302));
#30558=CARTESIAN_POINT('Ctrl Pts',(-0.266655038583099,0.0310102115966547,
-0.337501494106515));
#30559=CARTESIAN_POINT('Ctrl Pts',(-0.171139654349481,-0.206827854831415,
-0.32958103918073));
#30560=CARTESIAN_POINT('Ctrl Pts',(0.080373041066965,-0.256138082085956,
-0.321660584254943));
#30561=CARTESIAN_POINT('Ctrl Pts',(0.258624058202639,-0.0719731848942422,
-0.313740129329159));
#30562=CARTESIAN_POINT('Ctrl Pts',(0.201133932584729,0.177796749092968,
-0.305819674403371));
#30563=CARTESIAN_POINT('Ctrl Pts',(-0.0396939050912753,0.265501293261684,
-0.297899219477587));
#30564=CARTESIAN_POINT('Ctrl Pts',(-0.244339932723743,0.111195953620514,
-0.2899787645518));
#30565=CARTESIAN_POINT('Ctrl Pts',(-0.226265091458987,-0.144466782383002,
-0.282058309626015));
#30566=CARTESIAN_POINT('Ctrl Pts',(-0.00194497047620613,-0.268445078023149,
-0.274137854700228));
#30567=CARTESIAN_POINT('Ctrl Pts',(0.224148031056896,-0.147730169560283,
-0.266217399774443));
#30568=CARTESIAN_POINT('Ctrl Pts',(0.24592549692617,0.107643823727885,-0.258296944848656));
#30569=CARTESIAN_POINT('Ctrl Pts',(0.0435368195498848,0.264898260032731,
-0.250376489922871));
#30570=CARTESIAN_POINT('Ctrl Pts',(-0.198536563354313,0.180692489706502,
-0.242456034997085));
#30571=CARTESIAN_POINT('Ctrl Pts',(-0.259639789622127,-0.0682181975047813,
-0.234535580071299));
#30572=CARTESIAN_POINT('Ctrl Pts',(-0.0840760130734629,-0.254946596073716,
-0.226615125145513));
#30573=CARTESIAN_POINT('Ctrl Pts',(0.168124776812282,-0.209285934181618,
-0.218694670219728));
#30574=CARTESIAN_POINT('Ctrl Pts',(0.267076378351358,0.0271431567245319,
-0.210774215293941));
#30575=CARTESIAN_POINT('Ctrl Pts',(0.12258237362687,0.238830702574613,-0.202853760368156));
#30576=CARTESIAN_POINT('Ctrl Pts',(-0.133647983179599,0.232819156033741,
-0.19493330544237));
#30577=CARTESIAN_POINT('Ctrl Pts',(-0.268055457498088,0.0145881651932073,
-0.187012850516584));
#30578=CARTESIAN_POINT('Ctrl Pts',(-0.158124874603234,-0.216940237832751,
-0.179092395590798));
#30579=CARTESIAN_POINT('Ctrl Pts',(0.0959397799078894,-0.250723157032861,
-0.171171940665013));
#30580=CARTESIAN_POINT('Ctrl Pts',(0.262553354658447,-0.0559667668044061,
-0.163251485739226));
#30581=CARTESIAN_POINT('Ctrl Pts',(0.189844150667945,0.189804480457345,
-0.155331030813441));
#30582=CARTESIAN_POINT('Ctrl Pts',(-0.055911894283634,0.262565045579588,
-0.147410575887655));
#30583=CARTESIAN_POINT('Ctrl Pts',(-0.250703104374578,0.0959921740771708,
-0.139490120961869));
#30584=CARTESIAN_POINT('Ctrl Pts',(-0.216973273330174,-0.158079530835972,
-0.131569666036083));
#30585=CARTESIAN_POINT('Ctrl Pts',(0.0145321342700516,-0.268058505971775,
-0.123649211110297));
#30586=CARTESIAN_POINT('Ctrl Pts',(0.23279124095941,-0.133696625441738,
-0.115728756184511));
#30587=CARTESIAN_POINT('Ctrl Pts',(0.238856276268229,0.122532438246554,
-0.107808301258725));
#30588=CARTESIAN_POINT('Ctrl Pts',(0.0271990455951673,0.267070738870399,
-0.0998878463329397));
#30589=CARTESIAN_POINT('Ctrl Pts',(-0.209250935021787,0.16816843704613,
-0.0919673914071536));
#30590=CARTESIAN_POINT('Ctrl Pts',(-0.254963893066318,-0.0840225905618564,
-0.0840469364813679));
#30591=CARTESIAN_POINT('Ctrl Pts',(-0.068272966565161,-0.259625794146862,
-0.0761264815555819));
#30592=CARTESIAN_POINT('Ctrl Pts',(0.180651962505275,-0.198573814186845,
-0.0682060266297962));
#30593=CARTESIAN_POINT('Ctrl Pts',(0.264905513374514,0.0434804952224359,
-0.0602855717040101));
#30594=CARTESIAN_POINT('Ctrl Pts',(0.107698711478037,0.245904826017458,
-0.0523651167782246));
#30595=CARTESIAN_POINT('Ctrl Pts',(-0.147689963704326,0.224175421540604,
-0.0444446618524383));
#30596=CARTESIAN_POINT('Ctrl Pts',(-0.268432859279241,-0.00188226022256202,
-0.0365242069266527));
#30597=CARTESIAN_POINT('Ctrl Pts',(-0.144538048210606,-0.226247454230259,
-0.0286037520008667));
#30598=CARTESIAN_POINT('Ctrl Pts',(0.111190498414335,-0.244339288602387,
-0.0206832970750809));
#30599=CARTESIAN_POINT('Ctrl Pts',(0.265405974348622,-0.0397948740947594,
-0.0127628421492951));
#30600=CARTESIAN_POINT('Ctrl Pts',(0.178007129296782,0.201184176175435,
-0.00484238722350905));
#30601=CARTESIAN_POINT('Ctrl Pts',(-0.0722645024832365,0.258464596482291,
0.0030780677022766));
#30602=CARTESIAN_POINT('Ctrl Pts',(-0.194266559193884,0.140045363462362,
0.00835837098613384));
#30603=CARTESIAN_POINT('Ctrl Pts',(-0.216859401302392,0.0680976509636584,
0.0109985226280624));
#30604=CARTESIAN_POINT('Ctrl Pts',(0.126471106027295,-0.177287929553122,
-1.16365));
#30605=CARTESIAN_POINT('Ctrl Pts',(0.185290142270931,-0.135328453868889,
-1.16100984835807));
#30606=CARTESIAN_POINT('Ctrl Pts',(0.25689562471139,0.0109872606886212,
-1.15572954507421));
#30607=CARTESIAN_POINT('Ctrl Pts',(0.130348081000917,0.221923062878552,
-1.14780909014843));
#30608=CARTESIAN_POINT('Ctrl Pts',(-0.115118491958846,0.229917045457789,
-1.13988863522264));
#30609=CARTESIAN_POINT('Ctrl Pts',(-0.255597470383498,0.0286658565984495,
-1.13196818029686));
#30610=CARTESIAN_POINT('Ctrl Pts',(-0.163122903762403,-0.198886145851415,
-1.12404772537107));
#30611=CARTESIAN_POINT('Ctrl Pts',(0.0780566987792774,-0.245059402025012,
-1.11612727044528));
#30612=CARTESIAN_POINT('Ctrl Pts',(0.248078039310978,-0.0679032867325597,
-1.1082068155195));
#30613=CARTESIAN_POINT('Ctrl Pts',(0.191975348375761,0.171172964635631,
-1.10028636059371));
#30614=CARTESIAN_POINT('Ctrl Pts',(-0.0391190265108933,0.254208440109437,
-1.09236590566793));
#30615=CARTESIAN_POINT('Ctrl Pts',(-0.234554442114105,0.10553459470797,
-1.08444545074214));
#30616=CARTESIAN_POINT('Ctrl Pts',(-0.216189276575422,-0.139339830996314,
-1.07652499581635));
#30617=CARTESIAN_POINT('Ctrl Pts',(-0.000762821507371324,-0.25720122800503,
-1.06860454089057));
#30618=CARTESIAN_POINT('Ctrl Pts',(0.215358791521507,-0.140619426360152,
-1.06068408596478));
#30619=CARTESIAN_POINT('Ctrl Pts',(0.235176530521566,0.104140400581766,
-1.052763631039));
#30620=CARTESIAN_POINT('Ctrl Pts',(0.0406259830504325,0.253973834313976,
-1.04484317611321));
#30621=CARTESIAN_POINT('Ctrl Pts',(-0.190955957963633,0.172305046433272,
-1.03692272118743));
#30622=CARTESIAN_POINT('Ctrl Pts',(-0.248477632908984,-0.0664234085722272,
-1.02900226626164));
#30623=CARTESIAN_POINT('Ctrl Pts',(-0.0795068333803697,-0.244605521341649,
-1.02108181133586));
#30624=CARTESIAN_POINT('Ctrl Pts',(0.161936074723358,-0.199824697090791,
-1.01316135641007));
#30625=CARTESIAN_POINT('Ctrl Pts',(0.25577092546644,0.0271004554068604,
-1.00524090148428));
#30626=CARTESIAN_POINT('Ctrl Pts',(0.116465321567834,0.229322980077886,
-0.997320446558497));
#30627=CARTESIAN_POINT('Ctrl Pts',(-0.129000815316647,0.222512899840908,
-0.98939999163271));
#30628=CARTESIAN_POINT('Ctrl Pts',(-0.25688005885963,0.0128777379999474,
-0.981479536706925));
#30629=CARTESIAN_POINT('Ctrl Pts',(-0.15060785073702,-0.208495745752166,
-0.973559081781138));
#30630=CARTESIAN_POINT('Ctrl Pts',(0.092946507651719,-0.239821073941797,
-0.965638626855354));
#30631=CARTESIAN_POINT('Ctrl Pts',(0.251778214672948,-0.05254456561971,
-0.957718171929568));
#30632=CARTESIAN_POINT('Ctrl Pts',(0.181108905951714,0.182627393722108,
-0.949797717003781));
#30633=CARTESIAN_POINT('Ctrl Pts',(-0.0546448916053246,0.251330731481492,
-0.941877262077996));
#30634=CARTESIAN_POINT('Ctrl Pts',(-0.240588747733507,0.090940943607816,
-0.93395680715221));
#30635=CARTESIAN_POINT('Ctrl Pts',(-0.207231017151944,-0.1523433828229,
-0.926036352226423));
#30636=CARTESIAN_POINT('Ctrl Pts',(0.0150220433400717,-0.256763585765983,
-0.918115897300639));
#30637=CARTESIAN_POINT('Ctrl Pts',(0.22358220268487,-0.127138504801763,
-0.910195442374852));
#30638=CARTESIAN_POINT('Ctrl Pts',(0.228342590551659,0.118375935480206,
-0.902274987449066));
#30639=CARTESIAN_POINT('Ctrl Pts',(0.0249640155933997,0.255988278415915,
-0.894354532523281));
#30640=CARTESIAN_POINT('Ctrl Pts',(-0.201169772490191,0.160262046027745,
-0.886434077597493));
#30641=CARTESIAN_POINT('Ctrl Pts',(-0.243933179705436,-0.0815463340657517,
-0.87851362267171));
#30642=CARTESIAN_POINT('Ctrl Pts',(-0.0643464817567947,-0.249023555203761,
-0.870593167745921));
#30643=CARTESIAN_POINT('Ctrl Pts',(0.173893356378981,-0.189510689323927,
-0.862672712820138));
#30644=CARTESIAN_POINT('Ctrl Pts',(0.253625827354345,0.042745063570017,
-0.85475225789435));
#30645=CARTESIAN_POINT('Ctrl Pts',(0.102173145688224,0.236037812777863,
-0.846831802968565));
#30646=CARTESIAN_POINT('Ctrl Pts',(-0.142412457526902,0.214177245994829,
-0.838911348042779));
#30647=CARTESIAN_POINT('Ctrl Pts',(-0.257186179693303,-0.00291028100810552,
-0.830990893116994));
#30648=CARTESIAN_POINT('Ctrl Pts',(-0.137529414910091,-0.217345027077388,
-0.823070438191206));
#30649=CARTESIAN_POINT('Ctrl Pts',(0.107488237249403,-0.233665315384629,
-0.815149983265423));
#30650=CARTESIAN_POINT('Ctrl Pts',(0.254528152697761,-0.0369948678203813,
-0.807229528339635));
#30651=CARTESIAN_POINT('Ctrl Pts',(0.169560427414887,0.193397161860414,
-0.79930907341385));
#30652=CARTESIAN_POINT('Ctrl Pts',(-0.0699651112530573,0.247503704958389,
-0.791388618488063));
#30653=CARTESIAN_POINT('Ctrl Pts',(-0.245716013507421,0.0760055357641992,
-0.783468163562279));
#30654=CARTESIAN_POINT('Ctrl Pts',(-0.197491720957168,-0.164773240892319,
-0.775547708636491));
#30655=CARTESIAN_POINT('Ctrl Pts',(0.0307503329195962,-0.255357823036844,
-0.767627253710707));
#30656=CARTESIAN_POINT('Ctrl Pts',(0.230962826542383,-0.113178502889618,
-0.759706798784921));
#30657=CARTESIAN_POINT('Ctrl Pts',(0.220647958398849,0.132165348012261,
-0.751786343859134));
#30658=CARTESIAN_POINT('Ctrl Pts',(0.00920794273158324,0.257037768725599,
-0.743865888933349));
#30659=CARTESIAN_POINT('Ctrl Pts',(-0.210625301922338,0.147614982135642,
-0.735945434007564));
#30660=CARTESIAN_POINT('Ctrl Pts',(-0.238469256356832,-0.096361893575216,
-0.728024979081776));
#30661=CARTESIAN_POINT('Ctrl Pts',(-0.0489435840216807,-0.252502923436333,
-0.720104524155992));
#30662=CARTESIAN_POINT('Ctrl Pts',(0.18519517074638,-0.178482350648465,
-0.712184069230205));
#30663=CARTESIAN_POINT('Ctrl Pts',(0.250524722350552,0.0582285518621306,
-0.70426361430442));
#30664=CARTESIAN_POINT('Ctrl Pts',(0.0874958422396386,0.241862932983866,
-0.696343159378634));
#30665=CARTESIAN_POINT('Ctrl Pts',(-0.155287295766334,0.205034281363778,
-0.688422704452848));
#30666=CARTESIAN_POINT('Ctrl Pts',(-0.256522873141319,-0.0186873303632409,
-0.680502249527062));
#30667=CARTESIAN_POINT('Ctrl Pts',(-0.12393258111715,-0.225375056513412,
-0.672581794601276));
#30668=CARTESIAN_POINT('Ctrl Pts',(0.121624804919859,-0.226628788085249,
-0.664661339675491));
#30669=CARTESIAN_POINT('Ctrl Pts',(0.256318682363535,-0.0213057229917977,
-0.656740884749704));
#30670=CARTESIAN_POINT('Ctrl Pts',(0.157372814497323,0.203437946357048,
-0.648820429823919));
#30671=CARTESIAN_POINT('Ctrl Pts',(-0.0850216071723404,0.242743747755972,
-0.640899974898132));
#30672=CARTESIAN_POINT('Ctrl Pts',(-0.249917087046534,0.0607836356510322,
-0.632979519972347));
#30673=CARTESIAN_POINT('Ctrl Pts',(-0.187008007269756,-0.176582009213218,
-0.625059065046561));
#30674=CARTESIAN_POINT('Ctrl Pts',(0.046362713408588,-0.252989524617473,
-0.617138610120775));
#30675=CARTESIAN_POINT('Ctrl Pts',(0.237472868244547,-0.0987918903984044,
-0.609218155194989));
#30676=CARTESIAN_POINT('Ctrl Pts',(0.212121624547043,0.145456581701572,
-0.601297700269203));
#30677=CARTESIAN_POINT('Ctrl Pts',(-0.00658283818582227,0.257118391022893,
-0.593377245343417));
#30678=CARTESIAN_POINT('Ctrl Pts',(-0.21928690866101,0.134411504160469,
-0.585456790417632));
#30679=CARTESIAN_POINT('Ctrl Pts',(-0.2321064564127,-0.110814230369215,
-0.577536335491846));
#30680=CARTESIAN_POINT('Ctrl Pts',(-0.033356200274203,-0.255030517123049,
-0.569615880566061));
#30681=CARTESIAN_POINT('Ctrl Pts',(0.195798917752269,-0.166781247650396,
-0.561695425640274));
#30682=CARTESIAN_POINT('Ctrl Pts',(0.246479299353905,0.0734925557508373,
-0.553774970714489));
#30683=CARTESIAN_POINT('Ctrl Pts',(0.0724887354193506,0.246776384603724,
-0.545854515788701));
#30684=CARTESIAN_POINT('Ctrl Pts',(-0.167576800206862,0.195118468611283,
-0.537934060862918));
#30685=CARTESIAN_POINT('Ctrl Pts',(-0.254892639403815,-0.0343939404334457,
-0.53001360593713));
#30686=CARTESIAN_POINT('Ctrl Pts',(-0.109868600748205,-0.232555566113592,
-0.522093151011346));
#30687=CARTESIAN_POINT('Ctrl Pts',(0.135302924854754,-0.21873801518376,
-0.514172696085558));
#30688=CARTESIAN_POINT('Ctrl Pts',(0.257143054512441,-0.0055362692125341,
-0.506252241159774));
#30689=CARTESIAN_POINT('Ctrl Pts',(0.144592006708923,0.212711899894362,
-0.498331786233987));
#30690=CARTESIAN_POINT('Ctrl Pts',(-0.0997576260038526,0.237068801858992,
-0.490411331308202));
#30691=CARTESIAN_POINT('Ctrl Pts',(-0.253176132989307,0.0453326201025579,
-0.482490876382416));
#30692=CARTESIAN_POINT('Ctrl Pts',(-0.175819392986446,-0.187725176283469,
-0.474570421456629));
#30693=CARTESIAN_POINT('Ctrl Pts',(0.0618003361169582,-0.249667617476944,
-0.466649966530844));
#30694=CARTESIAN_POINT('Ctrl Pts',(0.243087789097186,-0.0840328956577408,
-0.458729511605058));
#30695=CARTESIAN_POINT('Ctrl Pts',(0.202795727822344,0.158199537097262,
-0.450809056679272));
#30696=CARTESIAN_POINT('Ctrl Pts',(-0.0223488060129853,0.256229841413087,
-0.442888601753486));
#30697=CARTESIAN_POINT('Ctrl Pts',(-0.227121943987874,0.120701380770689,
-0.4349681468277));
#30698=CARTESIAN_POINT('Ctrl Pts',(-0.22486876355983,-0.124848868380357,
-0.427047691901915));
#30699=CARTESIAN_POINT('Ctrl Pts',(-0.0176430849829593,-0.256596808852072,
-0.419127236976129));
#30700=CARTESIAN_POINT('Ctrl Pts',(0.205664628051519,-0.154451486005192,
-0.411206782050343));
#30701=CARTESIAN_POINT('Ctrl Pts',(0.241504807022057,0.0884795397028073,
-0.403286327124557));
#30702=CARTESIAN_POINT('Ctrl Pts',(0.0572083924230321,0.250759647066977,
-0.395365872198771));
#30703=CARTESIAN_POINT('Ctrl Pts',(-0.179234647275871,0.184467184010264,
-0.387445417272985));
#30704=CARTESIAN_POINT('Ctrl Pts',(-0.252301623419445,-0.0499709073431182,
-0.379524962347199));
#30705=CARTESIAN_POINT('Ctrl Pts',(-0.0953904860153474,-0.238859489948667,
-0.371604507421413));
#30706=CARTESIAN_POINT('Ctrl Pts',(0.148471039289085,-0.210022739847858,
-0.363684052495628));
#30707=CARTESIAN_POINT('Ctrl Pts',(0.256998161788665,0.0102540527612222,
-0.355763597569842));
#30708=CARTESIAN_POINT('Ctrl Pts',(0.13126617952173,0.221184065598206,-0.347843142644056));
#30709=CARTESIAN_POINT('Ctrl Pts',(-0.11411762238027,0.230500258184359,
-0.33992268771827));
#30710=CARTESIAN_POINT('Ctrl Pts',(-0.255480866816693,0.0297107295664827,
-0.332002232792484));
#30711=CARTESIAN_POINT('Ctrl Pts',(-0.163968052027973,-0.198160739489272,
-0.324081777866699));
#30712=CARTESIAN_POINT('Ctrl Pts',(0.0770050110794473,-0.245404623080814,
-0.316161322940912));
#30713=CARTESIAN_POINT('Ctrl Pts',(0.247786424439417,-0.0689571506394352,
-0.308240868015127));
#30714=CARTESIAN_POINT('Ctrl Pts',(0.192705420891506,0.170346181406604,
-0.300320413089341));
#30715=CARTESIAN_POINT('Ctrl Pts',(-0.038030533133535,0.254375469159979,
-0.292399958163555));
#30716=CARTESIAN_POINT('Ctrl Pts',(-0.234100874830238,0.106536290363869,
-0.284479503237769));
#30717=CARTESIAN_POINT('Ctrl Pts',(-0.216783459271804,-0.138412905998497,
-0.276559048311983));
#30718=CARTESIAN_POINT('Ctrl Pts',(-0.00186346654402013,-0.257195894705197,
-0.268638593386197));
#30719=CARTESIAN_POINT('Ctrl Pts',(0.214755114225321,-0.141539541029435,
-0.260718138460412));
#30720=CARTESIAN_POINT('Ctrl Pts',(0.235619996010104,0.103133012372812,
-0.252797683534625));
#30721=CARTESIAN_POINT('Ctrl Pts',(0.0417124103716506,0.25379770602124,
-0.24487722860884));
#30722=CARTESIAN_POINT('Ctrl Pts',(-0.190216894344415,0.173120576092536,
-0.236956773683054));
#30723=CARTESIAN_POINT('Ctrl Pts',(-0.248759591662818,-0.0653595158891499,
-0.229036318757268));
#30724=CARTESIAN_POINT('Ctrl Pts',(-0.0805528101499051,-0.244263066255845,
-0.221115863831482));
#30725=CARTESIAN_POINT('Ctrl Pts',(0.161079512847755,-0.200515813094597,
-0.213195408905696));
#30726=CARTESIAN_POINT('Ctrl Pts',(0.255884550354012,0.0260057235181914,
-0.20527495397991));
#30727=CARTESIAN_POINT('Ctrl Pts',(0.117445562765472,0.228822508812962,
-0.197354499054125));
#30728=CARTESIAN_POINT('Ctrl Pts',(-0.128047468266331,0.223062875957976,
-0.189434044128339));
#30729=CARTESIAN_POINT('Ctrl Pts',(-0.256822601217097,0.0139768485479575,
-0.181513589202553));
#30730=CARTESIAN_POINT('Ctrl Pts',(-0.151498656254814,-0.207849363370115,
-0.173593134276767));
#30731=CARTESIAN_POINT('Ctrl Pts',(0.0919194261743976,-0.240216610307221,
-0.165672679350981));
#30732=CARTESIAN_POINT('Ctrl Pts',(0.25155106383961,-0.0536214810419249,
-0.157752224425195));
#30733=CARTESIAN_POINT('Ctrl Pts',(0.181888736963096,0.181850729131537,
-0.149831769499409));
#30734=CARTESIAN_POINT('Ctrl Pts',(-0.0535689079525661,0.251562264853035,
-0.141911314573623));
#30735=CARTESIAN_POINT('Ctrl Pts',(-0.240197397955011,0.0919696247675137,
-0.133990859647838));
#30736=CARTESIAN_POINT('Ctrl Pts',(-0.207881014515963,-0.151455212616823,
-0.126070404722052));
#30737=CARTESIAN_POINT('Ctrl Pts',(0.0139231655990339,-0.256825521944582,
-0.118149949796266));
#30738=CARTESIAN_POINT('Ctrl Pts',(0.223036130664036,-0.128094072175867,
-0.11022949487048));
#30739=CARTESIAN_POINT('Ctrl Pts',(0.228847010841678,0.117397719925839,
-0.102309039944694));
#30740=CARTESIAN_POINT('Ctrl Pts',(0.0260592703673014,0.255879147195341,
-0.0943885850189083));
#30741=CARTESIAN_POINT('Ctrl Pts',(-0.200482280573558,0.161121343500753,
-0.0864681300931226));
#30742=CARTESIAN_POINT('Ctrl Pts',(-0.244279638418466,-0.0805016263071196,
-0.0785476751673364));
#30743=CARTESIAN_POINT('Ctrl Pts',(-0.0654119898536204,-0.248746182667544,
-0.0706272202415509));
#30744=CARTESIAN_POINT('Ctrl Pts',(0.173081747182517,-0.190252584181875,
-0.0627067653157647));
#30745=CARTESIAN_POINT('Ctrl Pts',(0.253804655411944,0.0416584463135328,
-0.0547863103899791));
#30746=CARTESIAN_POINT('Ctrl Pts',(0.103185600053364,0.235600191315231,
-0.0468658554641932));
#30747=CARTESIAN_POINT('Ctrl Pts',(-0.141501019998722,0.214781356911593,
-0.0389454005384072));
#30748=CARTESIAN_POINT('Ctrl Pts',(-0.257184187987403,-0.00180338416176167,
-0.0310249456126215));
#30749=CARTESIAN_POINT('Ctrl Pts',(-0.138481185433633,-0.216766561130641,
-0.0231044906868355));
#30750=CARTESIAN_POINT('Ctrl Pts',(0.106531063757949,-0.234100257700769,
-0.0151840357610497));
#30751=CARTESIAN_POINT('Ctrl Pts',(0.254284144583244,-0.0381272710338155,
-0.00726358083526386));
#30752=CARTESIAN_POINT('Ctrl Pts',(0.170547745633993,0.19275355902598,0.000656874090522184));
#30753=CARTESIAN_POINT('Ctrl Pts',(-0.0692362605731931,0.247633644957901,
0.00857732901630782));
#30754=CARTESIAN_POINT('Ctrl Pts',(-0.186125824586221,0.134176766511289,
0.0138576323001651));
#30755=CARTESIAN_POINT('Ctrl Pts',(-0.20777191429225,0.0652440208473855,
0.0164977839420937));
#30756=CARTESIAN_POINT('Ctrl Pts',(0.157411390703589,0.150985252349406,
2.77555756156289E-17));
#30757=CARTESIAN_POINT('Ctrl Pts',(0.153564701611678,0.155598258518773,
1.79071970638144E-17));
#30758=CARTESIAN_POINT('Ctrl Pts',(0.149524200953796,0.160033000704482,
-1.97347420389862E-16));
#30759=CARTESIAN_POINT('Ctrl Pts',(0.145294941952413,0.164273870340422,
-1.45716771982052E-16));
#30760=CARTESIAN_POINT('Ctrl Pts',(0.13714601219612,0.172445171449571,-4.59119247969748E-17));
#30761=CARTESIAN_POINT('Ctrl Pts',(0.128297493209746,0.179897878181489,
-8.12010810131507E-18));
#30762=CARTESIAN_POINT('Ctrl Pts',(0.118867987330782,0.186618959304511,
-4.5102810375397E-17));
#30763=CARTESIAN_POINT('Ctrl Pts',(0.114918429711642,0.189434090606089,
-6.05930508416384E-17));
#30764=CARTESIAN_POINT('Ctrl Pts',(0.110867035362717,0.192120070666577,
6.04783058210693E-17));
#30765=CARTESIAN_POINT('Ctrl Pts',(0.106733791498232,0.194668718081002,
6.93889390390723E-18));
#30766=CARTESIAN_POINT('Ctrl Pts',(0.0951061479421179,0.201838574169047,
-1.4367820452717E-16));
#30767=CARTESIAN_POINT('Ctrl Pts',(0.0828107346625941,0.20794034750507,
1.36988496431349E-16));
#30768=CARTESIAN_POINT('Ctrl Pts',(0.0700321885925319,0.212945356424772,
2.89698820488127E-16));
#30769=CARTESIAN_POINT('Ctrl Pts',(0.0649061281753037,0.214953094861562,
3.50957929557155E-16));
#30770=CARTESIAN_POINT('Ctrl Pts',(0.0596992770508872,0.216784433784475,
1.31329437058139E-16));
#30771=CARTESIAN_POINT('Ctrl Pts',(0.0544460276382488,0.218429702201119,
1.26634813746307E-16));
#30772=CARTESIAN_POINT('Ctrl Pts',(0.0403476443297082,0.222845183546339,
1.14035640598315E-16));
#30773=CARTESIAN_POINT('Ctrl Pts',(0.0258845556478006,0.225938110725585,
4.51833798814228E-17));
#30774=CARTESIAN_POINT('Ctrl Pts',(0.011276871154686,0.227669918440373,
-8.32667268468867E-17));
#30775=CARTESIAN_POINT('Ctrl Pts',(0.00107476123702629,0.228879425167524,
-1.7297718769337E-16));
#30776=CARTESIAN_POINT('Ctrl Pts',(-0.00919870048170219,0.229424155614405,
-2.66449797732721E-16));
#30777=CARTESIAN_POINT('Ctrl Pts',(-0.0194725016422591,0.229276419562986,
-2.68882138776405E-16));
#30778=CARTESIAN_POINT('Ctrl Pts',(-0.0236251828733368,0.229216704495672,
-2.69865293583651E-16));
#30779=CARTESIAN_POINT('Ctrl Pts',(-0.0277781740641179,0.229043424833214,
-8.41623659136518E-17));
#30780=CARTESIAN_POINT('Ctrl Pts',(-0.031911729017349,0.22875596618419,
-8.84708972748172E-17));
#30781=CARTESIAN_POINT('Ctrl Pts',(-0.0422252418762031,0.228038736461434,
-9.92209886849774E-17));
#30782=CARTESIAN_POINT('Ctrl Pts',(-0.0524404675808494,0.226611656750976,
-3.83662481248865E-16));
#30783=CARTESIAN_POINT('Ctrl Pts',(-0.0624850909091108,0.224457085590244,
-3.83373888190874E-16));
#30784=CARTESIAN_POINT('Ctrl Pts',(-0.0721327246316351,0.222387668678475,
-3.83096701080181E-16));
#30785=CARTESIAN_POINT('Ctrl Pts',(-0.0816232357754141,0.219647153966434,
-9.52791738662464E-17));
#30786=CARTESIAN_POINT('Ctrl Pts',(-0.0909164539954311,0.216284339764173,
-1.27502175484295E-16));
#30787=CARTESIAN_POINT('Ctrl Pts',(-0.0960519283334126,0.214426033456255,
-1.45308751633104E-16));
#30788=CARTESIAN_POINT('Ctrl Pts',(-0.101127127636006,0.212377488573957,
2.08088708794294E-16));
#30789=CARTESIAN_POINT('Ctrl Pts',(-0.10613488128436,0.210145550644494,
2.45463371850718E-16));
#30790=CARTESIAN_POINT('Ctrl Pts',(-0.110154437304024,0.208354048871471,
2.754627612817E-16));
#30791=CARTESIAN_POINT('Ctrl Pts',(-0.11413142148668,0.206443620358008,
1.33107852961981E-16));
#30792=CARTESIAN_POINT('Ctrl Pts',(-0.118046763621651,0.204426094738635,
1.17093834628434E-16));
#30793=CARTESIAN_POINT('Ctrl Pts',(-0.131295948505429,0.197598959582277,
6.29037581755335E-17));
#30794=CARTESIAN_POINT('Ctrl Pts',(-0.143882118085797,0.189531964554253,
-2.12688715064594E-18));
#30795=CARTESIAN_POINT('Ctrl Pts',(-0.155672563194254,0.180388335621176,
-2.18575157973078E-16));
#30796=CARTESIAN_POINT('Ctrl Pts',(-0.161475748336318,0.175887897250879,
-3.25109676195897E-16));
#30797=CARTESIAN_POINT('Ctrl Pts',(-0.167085969791737,0.171125853649587,
-2.08309637886367E-16));
#30798=CARTESIAN_POINT('Ctrl Pts',(-0.172485522512255,0.166117669875527,
-1.88651178012478E-16));
#30799=CARTESIAN_POINT('Ctrl Pts',(-0.176399951057423,0.162486965900707,
-1.74399694516081E-16));
#30800=CARTESIAN_POINT('Ctrl Pts',(-0.18020363364379,0.158726847330799,
-2.2547246652764E-17));
#30801=CARTESIAN_POINT('Ctrl Pts',(-0.183889191084364,0.154842509473871,
-1.99493199737333E-17));
#30802=CARTESIAN_POINT('Ctrl Pts',(-0.187043738235936,0.151517821927989,
-1.77256991680701E-17));
#30803=CARTESIAN_POINT('Ctrl Pts',(-0.19010667756743,0.148107231803098,
-2.31285918917368E-16));
#30804=CARTESIAN_POINT('Ctrl Pts',(-0.193068825214573,0.1446211636127,-2.34621350125863E-16));
#30805=CARTESIAN_POINT('Ctrl Pts',(-0.203021696728538,0.132907909271241,
-2.45828461389825E-16));
#30806=CARTESIAN_POINT('Ctrl Pts',(-0.211858816472026,0.120324866147189,
-1.29773094504587E-16));
#30807=CARTESIAN_POINT('Ctrl Pts',(-0.219427486736791,0.107016492388279,
-1.84314369322536E-16));
#30808=CARTESIAN_POINT('Ctrl Pts',(-0.225471071905783,0.0963897524908907,
-2.27865591407372E-16));
#30809=CARTESIAN_POINT('Ctrl Pts',(-0.230705723677907,0.0852994432307312,
-6.22160315497662E-18));
#30810=CARTESIAN_POINT('Ctrl Pts',(-0.235034375322676,0.0738049111962042,
0.));
#30811=CARTESIAN_POINT('Origin',(0.429366365092022,-0.191166222245626,0.6));
#30812=CARTESIAN_POINT('',(0.429366365092022,-0.191166222245626,0.57));
#30813=CARTESIAN_POINT('',(0.4625355188348,-0.189897061104753,0.54));
#30814=CARTESIAN_POINT('Ctrl Pts',(0.429366365092022,-0.191166222245626,
0.57));
#30815=CARTESIAN_POINT('Ctrl Pts',(0.445438016905544,-0.190551267878399,
0.555567939963915));
#30816=CARTESIAN_POINT('Ctrl Pts',(0.4625355188348,-0.189897061104753,0.54));
#30817=CARTESIAN_POINT('',(0.429366365092022,-0.191166222245626,0.0200000000000001));
#30818=CARTESIAN_POINT('',(0.429366365092022,-0.191166222245626,0.6));
#30819=CARTESIAN_POINT('',(0.4625355188348,-0.189897061104753,0.05));
#30820=CARTESIAN_POINT('Ctrl Pts',(0.4625355188348,-0.189897061104753,0.05));
#30821=CARTESIAN_POINT('Ctrl Pts',(0.445438016905538,-0.190551267878399,
0.03443206003608));
#30822=CARTESIAN_POINT('Ctrl Pts',(0.429366365092022,-0.191166222245626,
0.0200000000000001));
#30823=CARTESIAN_POINT('',(0.4625355188348,-0.189897061104753,0.295));
#30824=CARTESIAN_POINT('Origin',(0.478549932784856,-0.250179858964726,0.6));
#30825=CARTESIAN_POINT('',(0.450617690513801,-0.216664941778795,0.54));
#30826=CARTESIAN_POINT('Ctrl Pts',(0.450617690513801,-0.216664941778795,
0.54));
#30827=CARTESIAN_POINT('Ctrl Pts',(0.439663399059283,-0.203521271916345,
0.555567939963915));
#30828=CARTESIAN_POINT('Ctrl Pts',(0.429366365092022,-0.191166222245626,
0.57));
#30829=CARTESIAN_POINT('',(0.450617690513801,-0.216664941778795,0.05));
#30830=CARTESIAN_POINT('',(0.450617690513801,-0.216664941778795,0.295));
#30831=CARTESIAN_POINT('Ctrl Pts',(0.429366365092022,-0.191166222245626,
0.0200000000000001));
#30832=CARTESIAN_POINT('Ctrl Pts',(0.439663399059267,-0.203521271916326,
0.0344320600360628));
#30833=CARTESIAN_POINT('Ctrl Pts',(0.450617690513801,-0.216664941778795,
0.0500000000000001));
#30834=CARTESIAN_POINT('Origin',(0.314491384988663,-0.349278067974375,0.6));
#30835=CARTESIAN_POINT('',(0.314491384988663,-0.349278067974375,0.57));
#30836=CARTESIAN_POINT('',(0.345309129066188,-0.361609741826117,0.54));
#30837=CARTESIAN_POINT('Ctrl Pts',(0.314491384988663,-0.349278067974375,
0.57));
#30838=CARTESIAN_POINT('Ctrl Pts',(0.329423693974679,-0.355253208912848,
0.555567939963926));
#30839=CARTESIAN_POINT('Ctrl Pts',(0.345309129066188,-0.361609741826117,
0.54));
#30840=CARTESIAN_POINT('',(0.314491384988663,-0.349278067974375,0.0200000000000001));
#30841=CARTESIAN_POINT('',(0.314491384988663,-0.349278067974375,0.6));
#30842=CARTESIAN_POINT('',(0.345309129066188,-0.361609741826117,0.05));
#30843=CARTESIAN_POINT('Ctrl Pts',(0.345309129066188,-0.361609741826117,
0.0500000000000001));
#30844=CARTESIAN_POINT('Ctrl Pts',(0.32942369397468,-0.355253208912848,
0.0344320600360752));
#30845=CARTESIAN_POINT('Ctrl Pts',(0.314491384988663,-0.349278067974375,
0.0200000000000001));
#30846=CARTESIAN_POINT('',(0.345309129066188,-0.361609741826117,0.295));
#30847=CARTESIAN_POINT('Origin',(0.335419801350288,-0.423194466955954,0.6));
#30848=CARTESIAN_POINT('',(0.323534173210961,-0.38121600014257,0.54));
#30849=CARTESIAN_POINT('Ctrl Pts',(0.323534173210961,-0.38121600014257,
0.54));
#30850=CARTESIAN_POINT('Ctrl Pts',(0.31887294216854,-0.364753148509481,
0.555567939963924));
#30851=CARTESIAN_POINT('Ctrl Pts',(0.314491384988663,-0.349278067974375,
0.57));
#30852=CARTESIAN_POINT('',(0.323534173210961,-0.38121600014257,0.05));
#30853=CARTESIAN_POINT('',(0.323534173210961,-0.38121600014257,0.295));
#30854=CARTESIAN_POINT('Ctrl Pts',(0.314491384988663,-0.349278067974375,
0.0200000000000001));
#30855=CARTESIAN_POINT('Ctrl Pts',(0.318872942168538,-0.364753148509474,
0.0344320600360705));
#30856=CARTESIAN_POINT('Ctrl Pts',(0.323534173210961,-0.38121600014257,
0.0500000000000001));
#30857=CARTESIAN_POINT('Origin',(0.145237987356225,-0.446996562658722,0.6));
#30858=CARTESIAN_POINT('',(0.145237987356225,-0.446996562658722,0.57));
#30859=CARTESIAN_POINT('',(0.168375653847077,-0.470796813064372,0.54));
#30860=CARTESIAN_POINT('Ctrl Pts',(0.145237987356225,-0.446996562658722,
0.57));
#30861=CARTESIAN_POINT('Ctrl Pts',(0.156449021635303,-0.458528642752187,
0.555567939963917));
#30862=CARTESIAN_POINT('Ctrl Pts',(0.168375653847077,-0.470796813064372,
0.54));
#30863=CARTESIAN_POINT('',(0.145237987356225,-0.446996562658722,0.0200000000000001));
#30864=CARTESIAN_POINT('',(0.145237987356225,-0.446996562658722,0.6));
#30865=CARTESIAN_POINT('',(0.168375653847077,-0.470796813064372,0.05));
#30866=CARTESIAN_POINT('Ctrl Pts',(0.168375653847077,-0.470796813064372,
0.05));
#30867=CARTESIAN_POINT('Ctrl Pts',(0.156449021635302,-0.458528642752186,
0.0344320600360816));
#30868=CARTESIAN_POINT('Ctrl Pts',(0.145237987356225,-0.446996562658722,
0.0200000000000001));
#30869=CARTESIAN_POINT('',(0.168375653847077,-0.470796813064372,0.295));
#30870=CARTESIAN_POINT('Origin',(0.134292539069021,-0.523034907009461,0.6));
#30871=CARTESIAN_POINT('',(0.140508658144255,-0.479851348843057,0.54));
#30872=CARTESIAN_POINT('Ctrl Pts',(0.140508658144255,-0.479851348843057,
0.54));
#30873=CARTESIAN_POINT('Ctrl Pts',(0.142946456707127,-0.462915892047004,
0.555567939963928));
#30874=CARTESIAN_POINT('Ctrl Pts',(0.145237987356225,-0.446996562658722,
0.57));
#30875=CARTESIAN_POINT('',(0.140508658144255,-0.479851348843057,0.05));
#30876=CARTESIAN_POINT('',(0.140508658144255,-0.479851348843057,0.295));
#30877=CARTESIAN_POINT('Ctrl Pts',(0.145237987356225,-0.446996562658722,
0.0200000000000001));
#30878=CARTESIAN_POINT('Ctrl Pts',(0.142946456707125,-0.46291589204702,
0.034432060036086));
#30879=CARTESIAN_POINT('Ctrl Pts',(0.140508658144255,-0.479851348843057,
0.05));
#30880=CARTESIAN_POINT('Origin',(-0.0491283777357971,-0.467425290823089,
0.6));
#30881=CARTESIAN_POINT('',(-0.0491283777357971,-0.467425290823089,0.57));
#30882=CARTESIAN_POINT('',(-0.0376715015669875,-0.498578838269023,0.54));
#30883=CARTESIAN_POINT('Ctrl Pts',(-0.0491283777357971,-0.467425290823089,
0.57));
#30884=CARTESIAN_POINT('Ctrl Pts',(-0.0435771078395689,-0.482520308657719,
0.555567939963922));
#30885=CARTESIAN_POINT('Ctrl Pts',(-0.0376715015669874,-0.498578838269023,
0.54));
#30886=CARTESIAN_POINT('',(-0.0491283777357971,-0.467425290823089,0.0200000000000001));
#30887=CARTESIAN_POINT('',(-0.0491283777357971,-0.467425290823089,0.6));
#30888=CARTESIAN_POINT('',(-0.0376715015669875,-0.498578838269023,0.05));
#30889=CARTESIAN_POINT('Ctrl Pts',(-0.0376715015669875,-0.498578838269023,
0.05));
#30890=CARTESIAN_POINT('Ctrl Pts',(-0.0435771078395687,-0.482520308657719,
0.0344320600360783));
#30891=CARTESIAN_POINT('Ctrl Pts',(-0.0491283777357971,-0.467425290823089,
0.0200000000000001));
#30892=CARTESIAN_POINT('',(-0.0376715015669875,-0.498578838269023,0.295));
#30893=CARTESIAN_POINT('Origin',(-0.0900551232266954,-0.532437860018073,
0.6));
#30894=CARTESIAN_POINT('',(-0.066812080396678,-0.495516040015929,0.54));
#30895=CARTESIAN_POINT('Ctrl Pts',(-0.066812080396678,-0.495516040015929,
0.54));
#30896=CARTESIAN_POINT('Ctrl Pts',(-0.0576967697467444,-0.481036272390762,
0.555567939963916));
#30897=CARTESIAN_POINT('Ctrl Pts',(-0.0491283777357971,-0.467425290823089,
0.57));
#30898=CARTESIAN_POINT('',(-0.066812080396678,-0.495516040015929,0.05));
#30899=CARTESIAN_POINT('',(-0.066812080396678,-0.495516040015929,0.295));
#30900=CARTESIAN_POINT('Ctrl Pts',(-0.0491283777357971,-0.467425290823089,
0.0200000000000001));
#30901=CARTESIAN_POINT('Ctrl Pts',(-0.057696769746745,-0.481036272390763,
0.0344320600360851));
#30902=CARTESIAN_POINT('Ctrl Pts',(-0.0668120803966779,-0.495516040015929,
0.05));
#30903=CARTESIAN_POINT('Origin',(-0.235,-0.407031939778686,0.6));
#30904=CARTESIAN_POINT('',(-0.235,-0.407031939778686,0.57));
#30905=CARTESIAN_POINT('',(-0.237204912125273,-0.440152052890409,0.54));
#30906=CARTESIAN_POINT('Ctrl Pts',(-0.235,-0.407031939778686,0.57));
#30907=CARTESIAN_POINT('Ctrl Pts',(-0.23606835948338,-0.423079829636952,
0.555567939963917));
#30908=CARTESIAN_POINT('Ctrl Pts',(-0.237204912125273,-0.440152052890409,
0.54));
#30909=CARTESIAN_POINT('',(-0.235,-0.407031939778686,0.0200000000000001));
#30910=CARTESIAN_POINT('',(-0.235,-0.407031939778686,0.6));
#30911=CARTESIAN_POINT('',(-0.237204912125273,-0.440152052890409,0.05));
#30912=CARTESIAN_POINT('Ctrl Pts',(-0.237204912125273,-0.440152052890409,
0.05));
#30913=CARTESIAN_POINT('Ctrl Pts',(-0.236068359483381,-0.423079829636958,
0.0344320600360886));
#30914=CARTESIAN_POINT('Ctrl Pts',(-0.235,-0.407031939778686,0.0200000000000001));
#30915=CARTESIAN_POINT('',(-0.237204912125273,-0.440152052890409,0.295));
#30916=CARTESIAN_POINT('Origin',(-0.298831436591406,-0.449777469983454,
0.6));
#30917=CARTESIAN_POINT('',(-0.26258040326833,-0.425501506248146,0.54));
#30918=CARTESIAN_POINT('Ctrl Pts',(-0.26258040326833,-0.425501506248146,
0.54));
#30919=CARTESIAN_POINT('Ctrl Pts',(-0.248363700552694,-0.415981111160794,
0.555567939963927));
#30920=CARTESIAN_POINT('Ctrl Pts',(-0.235,-0.407031939778686,0.57));
#30921=CARTESIAN_POINT('',(-0.26258040326833,-0.425501506248146,0.05));
#30922=CARTESIAN_POINT('',(-0.26258040326833,-0.425501506248146,0.295));
#30923=CARTESIAN_POINT('Ctrl Pts',(-0.235,-0.407031939778686,0.0200000000000001));
#30924=CARTESIAN_POINT('Ctrl Pts',(-0.248363700552699,-0.415981111160797,
0.0344320600360783));
#30925=CARTESIAN_POINT('Ctrl Pts',(-0.26258040326833,-0.425501506248146,
0.05));
#30926=CARTESIAN_POINT('Origin',(-0.380237987356225,-0.276259068577462,
0.6));
#30927=CARTESIAN_POINT('',(-0.380237987356225,-0.276259068577462,0.57));
#30928=CARTESIAN_POINT('',(-0.395723438438122,-0.305618978911176,0.54));
#30929=CARTESIAN_POINT('Ctrl Pts',(-0.380237987356225,-0.276259068577462,
0.57));
#30930=CARTESIAN_POINT('Ctrl Pts',(-0.387741247158797,-0.290485004512361,
0.555567939963918));
#30931=CARTESIAN_POINT('Ctrl Pts',(-0.395723438438122,-0.305618978911176,
0.54));
#30932=CARTESIAN_POINT('',(-0.380237987356225,-0.276259068577462,0.0200000000000001));
#30933=CARTESIAN_POINT('',(-0.380237987356225,-0.276259068577462,0.6));
#30934=CARTESIAN_POINT('',(-0.395723438438122,-0.305618978911176,0.05));
#30935=CARTESIAN_POINT('Ctrl Pts',(-0.395723438438122,-0.305618978911176,
0.0500000000000001));
#30936=CARTESIAN_POINT('Ctrl Pts',(-0.387741247158801,-0.290485004512368,
0.0344320600360894));
#30937=CARTESIAN_POINT('Ctrl Pts',(-0.380237987356225,-0.276259068577462,
0.0200000000000001));
#30938=CARTESIAN_POINT('',(-0.395723438438122,-0.305618978911176,0.295));
#30939=CARTESIAN_POINT('Origin',(-0.455937079771088,-0.289346469288658,
0.6));
#30940=CARTESIAN_POINT('',(-0.412946188946813,-0.281913896490228,0.54));
#30941=CARTESIAN_POINT('Ctrl Pts',(-0.412946188946813,-0.281913896490228,
0.54));
#30942=CARTESIAN_POINT('Ctrl Pts',(-0.39608629121971,-0.278999036741381,
0.555567939963921));
#30943=CARTESIAN_POINT('Ctrl Pts',(-0.380237987356225,-0.276259068577462,
0.57));
#30944=CARTESIAN_POINT('',(-0.412946188946813,-0.281913896490228,0.05));
#30945=CARTESIAN_POINT('',(-0.412946188946813,-0.281913896490228,0.295));
#30946=CARTESIAN_POINT('Ctrl Pts',(-0.380237987356225,-0.276259068577462,
0.0200000000000001));
#30947=CARTESIAN_POINT('Ctrl Pts',(-0.396086291219724,-0.278999036741383,
0.0344320600360921));
#30948=CARTESIAN_POINT('Ctrl Pts',(-0.412946188946813,-0.281913896490228,
0.05));
#30949=CARTESIAN_POINT('Origin',(-0.459729372344889,-0.097718494684347,
0.6));
#30950=CARTESIAN_POINT('',(-0.459729372344889,-0.097718494684347,0.57));
#30951=CARTESIAN_POINT('',(-0.485817787210443,-0.11824160701694,0.54));
#30952=CARTESIAN_POINT('Ctrl Pts',(-0.459729372344889,-0.097718494684347,
0.57));
#30953=CARTESIAN_POINT('Ctrl Pts',(-0.472370150681811,-0.107662683134163,
0.55556793996392));
#30954=CARTESIAN_POINT('Ctrl Pts',(-0.485817787210443,-0.11824160701694,
0.54));
#30955=CARTESIAN_POINT('',(-0.459729372344889,-0.097718494684347,0.0200000000000001));
#30956=CARTESIAN_POINT('',(-0.459729372344889,-0.097718494684347,0.6));
#30957=CARTESIAN_POINT('',(-0.485817787210443,-0.11824160701694,0.05));
#30958=CARTESIAN_POINT('Ctrl Pts',(-0.485817787210443,-0.11824160701694,
0.0500000000000001));
#30959=CARTESIAN_POINT('Ctrl Pts',(-0.472370150681806,-0.107662683134159,
0.0344320600360745));
#30960=CARTESIAN_POINT('Ctrl Pts',(-0.459729372344889,-0.097718494684347,
0.0200000000000001));
#30961=CARTESIAN_POINT('',(-0.485817787210443,-0.11824160701694,0.295));
#30962=CARTESIAN_POINT('Origin',(-0.534207059800014,-0.0788848354237023,
0.6));
#30963=CARTESIAN_POINT('',(-0.491909827058038,-0.0895808129218024,0.54));
#30964=CARTESIAN_POINT('Ctrl Pts',(-0.491909827058038,-0.0895808129218024,
0.54));
#30965=CARTESIAN_POINT('Ctrl Pts',(-0.475321963803841,-0.0937754942427008,
0.555567939963922));
#30966=CARTESIAN_POINT('Ctrl Pts',(-0.459729372344889,-0.097718494684347,
0.57));
#30967=CARTESIAN_POINT('',(-0.491909827058038,-0.0895808129218024,0.05));
#30968=CARTESIAN_POINT('',(-0.491909827058038,-0.0895808129218024,0.295));
#30969=CARTESIAN_POINT('Ctrl Pts',(-0.459729372344889,-0.097718494684347,
0.0200000000000001));
#30970=CARTESIAN_POINT('Ctrl Pts',(-0.475321963803826,-0.0937754942427046,
0.0344320600360648));
#30971=CARTESIAN_POINT('Ctrl Pts',(-0.491909827058038,-0.0895808129218024,
0.0500000000000001));
#30972=CARTESIAN_POINT('Origin',(0.47,0.,0.6));
#30973=CARTESIAN_POINT('',(0.47,0.,0.57));
#30974=CARTESIAN_POINT('',(0.499785315393603,0.0146505466422634,0.54));
#30975=CARTESIAN_POINT('Ctrl Pts',(0.47,0.,0.57));
#30976=CARTESIAN_POINT('Ctrl Pts',(0.484432060036079,0.00709871847614981,
0.555567939963921));
#30977=CARTESIAN_POINT('Ctrl Pts',(0.499785315393603,0.0146505466422635,
0.54));
#30978=CARTESIAN_POINT('',(0.47,0.,0.0200000000000001));
#30979=CARTESIAN_POINT('',(0.47,0.,0.6));
#30980=CARTESIAN_POINT('',(0.499785315393603,0.0146505466422634,0.05));
#30981=CARTESIAN_POINT('Ctrl Pts',(0.499785315393603,0.0146505466422634,
0.05));
#30982=CARTESIAN_POINT('Ctrl Pts',(0.484432060036085,0.00709871847615275,
0.0344320600360846));
#30983=CARTESIAN_POINT('Ctrl Pts',(0.47,0.,0.0200000000000001));
#30984=CARTESIAN_POINT('',(0.499785315393603,0.0146505466422634,0.295));
#30985=CARTESIAN_POINT('Origin',(0.538934433351267,-0.0339068805458292,
0.6));
#30986=CARTESIAN_POINT('',(0.499785315393603,-0.0146505466422634,0.54));
#30987=CARTESIAN_POINT('Ctrl Pts',(0.499785315393603,-0.0146505466422635,
0.54));
#30988=CARTESIAN_POINT('Ctrl Pts',(0.48443206003608,-0.00709871847615054,
0.55556793996392));
#30989=CARTESIAN_POINT('Ctrl Pts',(0.47,0.,0.57));
#30990=CARTESIAN_POINT('',(0.499785315393603,-0.0146505466422634,0.05));
#30991=CARTESIAN_POINT('',(0.499785315393603,-0.0146505466422634,0.295));
#30992=CARTESIAN_POINT('Ctrl Pts',(0.47,0.,0.0200000000000001));
#30993=CARTESIAN_POINT('Ctrl Pts',(0.484432060036087,-0.00709871847615401,
0.0344320600360872));
#30994=CARTESIAN_POINT('Ctrl Pts',(0.499785315393603,-0.0146505466422634,
0.05));
#30995=CARTESIAN_POINT('Origin',(-0.429366365092022,0.191166222245626,0.6));
#30996=CARTESIAN_POINT('',(-0.429366365092022,0.191166222245626,0.57));
#30997=CARTESIAN_POINT('',(-0.4625355188348,0.189897061104753,0.54));
#30998=CARTESIAN_POINT('Ctrl Pts',(-0.429366365092022,0.191166222245626,
0.57));
#30999=CARTESIAN_POINT('Ctrl Pts',(-0.445438016905526,0.190551267878399,
0.555567939963931));
#31000=CARTESIAN_POINT('Ctrl Pts',(-0.4625355188348,0.189897061104753,0.54));
#31001=CARTESIAN_POINT('',(-0.429366365092022,0.191166222245626,0.0200000000000001));
#31002=CARTESIAN_POINT('',(-0.429366365092022,0.191166222245626,0.6));
#31003=CARTESIAN_POINT('',(-0.4625355188348,0.189897061104753,0.05));
#31004=CARTESIAN_POINT('Ctrl Pts',(-0.4625355188348,0.189897061104753,0.05));
#31005=CARTESIAN_POINT('Ctrl Pts',(-0.445438016905521,0.1905512678784,0.0344320600360647));
#31006=CARTESIAN_POINT('Ctrl Pts',(-0.429366365092022,0.191166222245626,
0.0200000000000001));
#31007=CARTESIAN_POINT('',(-0.4625355188348,0.189897061104753,0.295));
#31008=CARTESIAN_POINT('Origin',(-0.478549932784856,0.250179858964725,0.6));
#31009=CARTESIAN_POINT('',(-0.450617690513801,0.216664941778795,0.54));
#31010=CARTESIAN_POINT('Ctrl Pts',(-0.450617690513801,0.216664941778795,
0.54));
#31011=CARTESIAN_POINT('Ctrl Pts',(-0.439663399059279,0.203521271916341,
0.55556793996392));
#31012=CARTESIAN_POINT('Ctrl Pts',(-0.429366365092022,0.191166222245626,
0.57));
#31013=CARTESIAN_POINT('',(-0.450617690513801,0.216664941778795,0.05));
#31014=CARTESIAN_POINT('',(-0.450617690513801,0.216664941778795,0.295));
#31015=CARTESIAN_POINT('Ctrl Pts',(-0.429366365092022,0.191166222245626,
0.0200000000000001));
#31016=CARTESIAN_POINT('Ctrl Pts',(-0.439663399059263,0.203521271916321,
0.0344320600360574));
#31017=CARTESIAN_POINT('Ctrl Pts',(-0.450617690513801,0.216664941778795,
0.0500000000000001));
#31018=CARTESIAN_POINT('Origin',(-0.314491384988663,0.349278067974375,0.6));
#31019=CARTESIAN_POINT('',(-0.314491384988663,0.349278067974375,0.57));
#31020=CARTESIAN_POINT('',(-0.345309129066188,0.361609741826117,0.54));
#31021=CARTESIAN_POINT('Ctrl Pts',(-0.314491384988663,0.349278067974375,
0.57));
#31022=CARTESIAN_POINT('Ctrl Pts',(-0.329423693974693,0.355253208912853,
0.555567939963912));
#31023=CARTESIAN_POINT('Ctrl Pts',(-0.345309129066188,0.361609741826117,
0.54));
#31024=CARTESIAN_POINT('',(-0.314491384988663,0.349278067974375,0.0200000000000001));
#31025=CARTESIAN_POINT('',(-0.314491384988663,0.349278067974375,0.6));
#31026=CARTESIAN_POINT('',(-0.345309129066188,0.361609741826117,0.05));
#31027=CARTESIAN_POINT('Ctrl Pts',(-0.345309129066188,0.361609741826117,
0.05));
#31028=CARTESIAN_POINT('Ctrl Pts',(-0.32942369397468,0.355253208912848,
0.0344320600360755));
#31029=CARTESIAN_POINT('Ctrl Pts',(-0.314491384988663,0.349278067974375,
0.0200000000000001));
#31030=CARTESIAN_POINT('',(-0.345309129066188,0.361609741826117,0.295));
#31031=CARTESIAN_POINT('Origin',(-0.335419801350288,0.423194466955954,0.6));
#31032=CARTESIAN_POINT('',(-0.323534173210961,0.38121600014257,0.54));
#31033=CARTESIAN_POINT('Ctrl Pts',(-0.323534173210961,0.38121600014257,
0.54));
#31034=CARTESIAN_POINT('Ctrl Pts',(-0.318872942168541,0.364753148509483,
0.555567939963922));
#31035=CARTESIAN_POINT('Ctrl Pts',(-0.314491384988663,0.349278067974375,
0.57));
#31036=CARTESIAN_POINT('',(-0.323534173210961,0.38121600014257,0.05));
#31037=CARTESIAN_POINT('',(-0.323534173210961,0.38121600014257,0.295));
#31038=CARTESIAN_POINT('Ctrl Pts',(-0.314491384988663,0.349278067974375,
0.0200000000000001));
#31039=CARTESIAN_POINT('Ctrl Pts',(-0.318872942168539,0.364753148509479,
0.0344320600360749));
#31040=CARTESIAN_POINT('Ctrl Pts',(-0.323534173210961,0.38121600014257,
0.0500000000000001));
#31041=CARTESIAN_POINT('Origin',(-0.145237987356225,0.446996562658722,0.6));
#31042=CARTESIAN_POINT('',(-0.145237987356225,0.446996562658722,0.57));
#31043=CARTESIAN_POINT('',(-0.168375653847077,0.470796813064372,0.54));
#31044=CARTESIAN_POINT('Ctrl Pts',(-0.145237987356225,0.446996562658722,
0.57));
#31045=CARTESIAN_POINT('Ctrl Pts',(-0.156449021635303,0.458528642752187,
0.555567939963918));
#31046=CARTESIAN_POINT('Ctrl Pts',(-0.168375653847077,0.470796813064372,
0.54));
#31047=CARTESIAN_POINT('',(-0.145237987356225,0.446996562658722,0.0200000000000001));
#31048=CARTESIAN_POINT('',(-0.145237987356225,0.446996562658722,0.6));
#31049=CARTESIAN_POINT('',(-0.168375653847077,0.470796813064372,0.05));
#31050=CARTESIAN_POINT('Ctrl Pts',(-0.168375653847077,0.470796813064372,
0.05));
#31051=CARTESIAN_POINT('Ctrl Pts',(-0.156449021635315,0.458528642752199,
0.0344320600360975));
#31052=CARTESIAN_POINT('Ctrl Pts',(-0.145237987356225,0.446996562658722,
0.0200000000000001));
#31053=CARTESIAN_POINT('',(-0.168375653847077,0.470796813064372,0.295));
#31054=CARTESIAN_POINT('Origin',(-0.134292539069022,0.523034907009461,0.6));
#31055=CARTESIAN_POINT('',(-0.140508658144256,0.479851348843057,0.54));
#31056=CARTESIAN_POINT('Ctrl Pts',(-0.140508658144256,0.479851348843057,
0.54));
#31057=CARTESIAN_POINT('Ctrl Pts',(-0.142946456707125,0.462915892047018,
0.555567939963916));
#31058=CARTESIAN_POINT('Ctrl Pts',(-0.145237987356225,0.446996562658722,
0.57));
#31059=CARTESIAN_POINT('',(-0.140508658144256,0.479851348843057,0.05));
#31060=CARTESIAN_POINT('',(-0.140508658144256,0.479851348843057,0.295));
#31061=CARTESIAN_POINT('Ctrl Pts',(-0.145237987356225,0.446996562658722,
0.0200000000000001));
#31062=CARTESIAN_POINT('Ctrl Pts',(-0.142946456707125,0.462915892047015,
0.034432060036082));
#31063=CARTESIAN_POINT('Ctrl Pts',(-0.140508658144256,0.479851348843057,
0.0500000000000001));
#31064=CARTESIAN_POINT('Origin',(0.0491283777357971,0.467425290823088,0.6));
#31065=CARTESIAN_POINT('',(0.0491283777357971,0.467425290823088,0.57));
#31066=CARTESIAN_POINT('',(0.0376715015669876,0.498578838269023,0.54));
#31067=CARTESIAN_POINT('Ctrl Pts',(0.0491283777357971,0.467425290823088,
0.57));
#31068=CARTESIAN_POINT('Ctrl Pts',(0.0435771078395701,0.482520308657716,
0.555567939963925));
#31069=CARTESIAN_POINT('Ctrl Pts',(0.0376715015669876,0.498578838269023,
0.54));
#31070=CARTESIAN_POINT('',(0.0491283777357971,0.467425290823088,0.02));
#31071=CARTESIAN_POINT('',(0.0491283777357971,0.467425290823088,0.6));
#31072=CARTESIAN_POINT('',(0.0376715015669876,0.498578838269023,0.05));
#31073=CARTESIAN_POINT('Ctrl Pts',(0.0376715015669877,0.498578838269023,
0.05));
#31074=CARTESIAN_POINT('Ctrl Pts',(0.0435771078395647,0.48252030865773,
0.0344320600360888));
#31075=CARTESIAN_POINT('Ctrl Pts',(0.0491283777357971,0.467425290823088,
0.02));
#31076=CARTESIAN_POINT('',(0.0376715015669876,0.498578838269023,0.295));
#31077=CARTESIAN_POINT('Origin',(0.0900551232266951,0.532437860018073,0.6));
#31078=CARTESIAN_POINT('',(0.0668120803966779,0.495516040015929,0.54));
#31079=CARTESIAN_POINT('Ctrl Pts',(0.0668120803966779,0.495516040015929,
0.54));
#31080=CARTESIAN_POINT('Ctrl Pts',(0.0576967697467487,0.481036272390768,
0.555567939963909));
#31081=CARTESIAN_POINT('Ctrl Pts',(0.0491283777357971,0.467425290823088,
0.57));
#31082=CARTESIAN_POINT('',(0.0668120803966779,0.495516040015929,0.05));
#31083=CARTESIAN_POINT('',(0.0668120803966779,0.495516040015929,0.295));
#31084=CARTESIAN_POINT('Ctrl Pts',(0.0491283777357971,0.467425290823088,
0.02));
#31085=CARTESIAN_POINT('Ctrl Pts',(0.0576967697467307,0.48103627239074,
0.034432060036061));
#31086=CARTESIAN_POINT('Ctrl Pts',(0.0668120803966779,0.495516040015929,
0.05));
#31087=CARTESIAN_POINT('Origin',(0.235,0.407031939778686,0.6));
#31088=CARTESIAN_POINT('',(0.235,0.407031939778686,0.57));
#31089=CARTESIAN_POINT('',(0.237204912125272,0.440152052890409,0.54));
#31090=CARTESIAN_POINT('Ctrl Pts',(0.235,0.407031939778686,0.57));
#31091=CARTESIAN_POINT('Ctrl Pts',(0.236068359483379,0.423079829636944,
0.555567939963924));
#31092=CARTESIAN_POINT('Ctrl Pts',(0.237204912125272,0.440152052890409,
0.54));
#31093=CARTESIAN_POINT('',(0.235,0.407031939778686,0.0200000000000001));
#31094=CARTESIAN_POINT('',(0.235,0.407031939778686,0.6));
#31095=CARTESIAN_POINT('',(0.237204912125272,0.440152052890409,0.05));
#31096=CARTESIAN_POINT('Ctrl Pts',(0.237204912125272,0.440152052890409,
0.05));
#31097=CARTESIAN_POINT('Ctrl Pts',(0.236068359483379,0.423079829636941,
0.0344320600360727));
#31098=CARTESIAN_POINT('Ctrl Pts',(0.235,0.407031939778686,0.0200000000000001));
#31099=CARTESIAN_POINT('',(0.237204912125272,0.440152052890409,0.295));
#31100=CARTESIAN_POINT('Origin',(0.298831436591406,0.449777469983454,0.6));
#31101=CARTESIAN_POINT('',(0.26258040326833,0.425501506248146,0.54));
#31102=CARTESIAN_POINT('Ctrl Pts',(0.26258040326833,0.425501506248146,0.54));
#31103=CARTESIAN_POINT('Ctrl Pts',(0.24836370055269,0.415981111160792,0.555567939963931));
#31104=CARTESIAN_POINT('Ctrl Pts',(0.235,0.407031939778686,0.57));
#31105=CARTESIAN_POINT('',(0.26258040326833,0.425501506248146,0.05));
#31106=CARTESIAN_POINT('',(0.26258040326833,0.425501506248146,0.295));
#31107=CARTESIAN_POINT('Ctrl Pts',(0.235,0.407031939778686,0.0200000000000001));
#31108=CARTESIAN_POINT('Ctrl Pts',(0.248363700552713,0.415981111160807,
0.0344320600360936));
#31109=CARTESIAN_POINT('Ctrl Pts',(0.26258040326833,0.425501506248146,0.05));
#31110=CARTESIAN_POINT('Origin',(0.380237987356225,0.276259068577462,0.6));
#31111=CARTESIAN_POINT('',(0.380237987356225,0.276259068577462,0.57));
#31112=CARTESIAN_POINT('',(0.395723438438122,0.305618978911176,0.54));
#31113=CARTESIAN_POINT('Ctrl Pts',(0.380237987356225,0.276259068577462,
0.57));
#31114=CARTESIAN_POINT('Ctrl Pts',(0.387741247158792,0.29048500451235,0.555567939963929));
#31115=CARTESIAN_POINT('Ctrl Pts',(0.395723438438122,0.305618978911176,
0.54));
#31116=CARTESIAN_POINT('',(0.380237987356225,0.276259068577462,0.0200000000000001));
#31117=CARTESIAN_POINT('',(0.380237987356225,0.276259068577462,0.6));
#31118=CARTESIAN_POINT('',(0.395723438438122,0.305618978911176,0.05));
#31119=CARTESIAN_POINT('Ctrl Pts',(0.395723438438122,0.305618978911176,
0.05));
#31120=CARTESIAN_POINT('Ctrl Pts',(0.387741247158797,0.290485004512361,
0.034432060036082));
#31121=CARTESIAN_POINT('Ctrl Pts',(0.380237987356225,0.276259068577462,
0.0200000000000001));
#31122=CARTESIAN_POINT('',(0.395723438438122,0.305618978911176,0.295));
#31123=CARTESIAN_POINT('Origin',(0.455937079771088,0.289346469288658,0.6));
#31124=CARTESIAN_POINT('',(0.412946188946813,0.281913896490228,0.54));
#31125=CARTESIAN_POINT('Ctrl Pts',(0.412946188946813,0.281913896490228,
0.54));
#31126=CARTESIAN_POINT('Ctrl Pts',(0.396086291219718,0.278999036741382,
0.555567939963914));
#31127=CARTESIAN_POINT('Ctrl Pts',(0.380237987356225,0.276259068577462,
0.57));
#31128=CARTESIAN_POINT('',(0.412946188946813,0.281913896490228,0.05));
#31129=CARTESIAN_POINT('',(0.412946188946813,0.281913896490228,0.295));
#31130=CARTESIAN_POINT('Ctrl Pts',(0.380237987356225,0.276259068577462,
0.0200000000000001));
#31131=CARTESIAN_POINT('Ctrl Pts',(0.396086291219722,0.278999036741383,
0.0344320600360903));
#31132=CARTESIAN_POINT('Ctrl Pts',(0.412946188946813,0.281913896490228,
0.05));
#31133=CARTESIAN_POINT('Origin',(0.459729372344889,0.0977184946843469,0.6));
#31134=CARTESIAN_POINT('',(0.459729372344889,0.0977184946843469,0.57));
#31135=CARTESIAN_POINT('',(0.485817787210443,0.11824160701694,0.54));
#31136=CARTESIAN_POINT('Ctrl Pts',(0.459729372344889,0.0977184946843469,
0.57));
#31137=CARTESIAN_POINT('Ctrl Pts',(0.472370150681809,0.107662683134161,
0.555567939963922));
#31138=CARTESIAN_POINT('Ctrl Pts',(0.485817787210443,0.11824160701694,0.54));
#31139=CARTESIAN_POINT('',(0.459729372344889,0.0977184946843469,0.0200000000000001));
#31140=CARTESIAN_POINT('',(0.459729372344889,0.0977184946843469,0.6));
#31141=CARTESIAN_POINT('',(0.485817787210443,0.11824160701694,0.05));
#31142=CARTESIAN_POINT('Ctrl Pts',(0.485817787210443,0.11824160701694,0.0500000000000001));
#31143=CARTESIAN_POINT('Ctrl Pts',(0.472370150681813,0.107662683134164,
0.034432060036082));
#31144=CARTESIAN_POINT('Ctrl Pts',(0.459729372344889,0.0977184946843469,
0.0200000000000001));
#31145=CARTESIAN_POINT('',(0.485817787210443,0.11824160701694,0.295));
#31146=CARTESIAN_POINT('Origin',(0.534207059800014,0.0788848354237023,0.6));
#31147=CARTESIAN_POINT('',(0.491909827058038,0.0895808129218023,0.54));
#31148=CARTESIAN_POINT('Ctrl Pts',(0.491909827058038,0.0895808129218023,
0.54));
#31149=CARTESIAN_POINT('Ctrl Pts',(0.475321963803841,0.0937754942427007,
0.555567939963922));
#31150=CARTESIAN_POINT('Ctrl Pts',(0.459729372344889,0.0977184946843469,
0.57));
#31151=CARTESIAN_POINT('',(0.491909827058038,0.0895808129218023,0.05));
#31152=CARTESIAN_POINT('',(0.491909827058038,0.0895808129218023,0.295));
#31153=CARTESIAN_POINT('Ctrl Pts',(0.459729372344889,0.0977184946843469,
0.0200000000000001));
#31154=CARTESIAN_POINT('Ctrl Pts',(0.475321963803834,0.0937754942427024,
0.0344320600360725));
#31155=CARTESIAN_POINT('Ctrl Pts',(0.491909827058038,0.0895808129218023,
0.05));
#31156=CARTESIAN_POINT('Origin',(0.429366365092022,0.191166222245626,0.6));
#31157=CARTESIAN_POINT('',(0.429366365092022,0.191166222245626,0.57));
#31158=CARTESIAN_POINT('',(0.450617690513801,0.216664941778795,0.54));
#31159=CARTESIAN_POINT('Ctrl Pts',(0.429366365092022,0.191166222245626,
0.57));
#31160=CARTESIAN_POINT('Ctrl Pts',(0.439663399059275,0.203521271916335,
0.555567939963926));
#31161=CARTESIAN_POINT('Ctrl Pts',(0.450617690513801,0.216664941778795,
0.54));
#31162=CARTESIAN_POINT('',(0.429366365092022,0.191166222245626,0.02));
#31163=CARTESIAN_POINT('',(0.429366365092022,0.191166222245626,0.6));
#31164=CARTESIAN_POINT('',(0.450617690513801,0.216664941778795,0.05));
#31165=CARTESIAN_POINT('Ctrl Pts',(0.450617690513801,0.216664941778795,
0.05));
#31166=CARTESIAN_POINT('Ctrl Pts',(0.439663399059281,0.203521271916343,
0.0344320600360824));
#31167=CARTESIAN_POINT('Ctrl Pts',(0.429366365092022,0.191166222245626,
0.02));
#31168=CARTESIAN_POINT('',(0.450617690513801,0.216664941778795,0.295));
#31169=CARTESIAN_POINT('Origin',(0.506132274325621,0.18822890555378,0.6));
#31170=CARTESIAN_POINT('',(0.4625355188348,0.189897061104753,0.54));
#31171=CARTESIAN_POINT('Ctrl Pts',(0.4625355188348,0.189897061104753,0.54));
#31172=CARTESIAN_POINT('Ctrl Pts',(0.445438016905532,0.190551267878399,
0.555567939963925));
#31173=CARTESIAN_POINT('Ctrl Pts',(0.429366365092022,0.191166222245626,
0.57));
#31174=CARTESIAN_POINT('',(0.4625355188348,0.189897061104753,0.05));
#31175=CARTESIAN_POINT('',(0.4625355188348,0.189897061104753,0.295));
#31176=CARTESIAN_POINT('Ctrl Pts',(0.429366365092022,0.191166222245626,
0.02));
#31177=CARTESIAN_POINT('Ctrl Pts',(0.445438016905514,0.1905512678784,0.0344320600360582));
#31178=CARTESIAN_POINT('Ctrl Pts',(0.4625355188348,0.189897061104753,0.05));
#31179=CARTESIAN_POINT('Origin',(0.314491384988663,0.349278067974375,0.6));
#31180=CARTESIAN_POINT('',(0.314491384988663,0.349278067974375,0.57));
#31181=CARTESIAN_POINT('',(0.323534173210961,0.38121600014257,0.54));
#31182=CARTESIAN_POINT('Ctrl Pts',(0.314491384988663,0.349278067974375,
0.57));
#31183=CARTESIAN_POINT('Ctrl Pts',(0.318872942168541,0.364753148509485,
0.55556793996392));
#31184=CARTESIAN_POINT('Ctrl Pts',(0.323534173210961,0.38121600014257,0.54));
#31185=CARTESIAN_POINT('',(0.314491384988663,0.349278067974375,0.0200000000000001));
#31186=CARTESIAN_POINT('',(0.314491384988663,0.349278067974375,0.6));
#31187=CARTESIAN_POINT('',(0.323534173210961,0.38121600014257,0.05));
#31188=CARTESIAN_POINT('Ctrl Pts',(0.323534173210961,0.38121600014257,0.05));
#31189=CARTESIAN_POINT('Ctrl Pts',(0.318872942168541,0.364753148509485,
0.03443206003608));
#31190=CARTESIAN_POINT('Ctrl Pts',(0.314491384988663,0.349278067974375,
0.0200000000000001));
#31191=CARTESIAN_POINT('',(0.323534173210961,0.38121600014257,0.295));
#31192=CARTESIAN_POINT('Origin',(0.385815247001714,0.377818203877217,0.6));
#31193=CARTESIAN_POINT('',(0.345309129066188,0.361609741826117,0.54));
#31194=CARTESIAN_POINT('Ctrl Pts',(0.345309129066188,0.361609741826117,
0.54));
#31195=CARTESIAN_POINT('Ctrl Pts',(0.32942369397469,0.355253208912852,0.555567939963916));
#31196=CARTESIAN_POINT('Ctrl Pts',(0.314491384988663,0.349278067974375,
0.57));
#31197=CARTESIAN_POINT('',(0.345309129066188,0.361609741826117,0.05));
#31198=CARTESIAN_POINT('',(0.345309129066188,0.361609741826117,0.295));
#31199=CARTESIAN_POINT('Ctrl Pts',(0.314491384988663,0.349278067974375,
0.0200000000000001));
#31200=CARTESIAN_POINT('Ctrl Pts',(0.329423693974684,0.355253208912849,
0.0344320600360788));
#31201=CARTESIAN_POINT('Ctrl Pts',(0.345309129066188,0.361609741826117,
0.0500000000000001));
#31202=CARTESIAN_POINT('Origin',(0.145237987356225,0.446996562658722,0.6));
#31203=CARTESIAN_POINT('',(0.145237987356225,0.446996562658722,0.57));
#31204=CARTESIAN_POINT('',(0.140508658144256,0.479851348843056,0.54));
#31205=CARTESIAN_POINT('Ctrl Pts',(0.145237987356225,0.446996562658722,
0.57));
#31206=CARTESIAN_POINT('Ctrl Pts',(0.142946456707127,0.462915892047007,
0.555567939963926));
#31207=CARTESIAN_POINT('Ctrl Pts',(0.140508658144256,0.479851348843057,
0.54));
#31208=CARTESIAN_POINT('',(0.145237987356225,0.446996562658722,0.0199999999999999));
#31209=CARTESIAN_POINT('',(0.145237987356225,0.446996562658722,0.6));
#31210=CARTESIAN_POINT('',(0.140508658144256,0.479851348843056,0.05));
#31211=CARTESIAN_POINT('Ctrl Pts',(0.140508658144256,0.479851348843057,
0.05));
#31212=CARTESIAN_POINT('Ctrl Pts',(0.142946456707125,0.462915892047022,
0.0344320600360881));
#31213=CARTESIAN_POINT('Ctrl Pts',(0.145237987356225,0.446996562658722,
0.0199999999999999));
#31214=CARTESIAN_POINT('',(0.140508658144256,0.479851348843056,0.295));
#31215=CARTESIAN_POINT('Origin',(0.198787258449726,0.502079302379656,0.6));
#31216=CARTESIAN_POINT('',(0.168375653847077,0.470796813064372,0.54));
#31217=CARTESIAN_POINT('Ctrl Pts',(0.168375653847077,0.470796813064372,
0.54));
#31218=CARTESIAN_POINT('Ctrl Pts',(0.156449021635289,0.458528642752173,
0.555567939963936));
#31219=CARTESIAN_POINT('Ctrl Pts',(0.145237987356225,0.446996562658722,
0.57));
#31220=CARTESIAN_POINT('',(0.168375653847077,0.470796813064372,0.05));
#31221=CARTESIAN_POINT('',(0.168375653847077,0.470796813064372,0.295));
#31222=CARTESIAN_POINT('Ctrl Pts',(0.145237987356225,0.446996562658722,
0.0199999999999999));
#31223=CARTESIAN_POINT('Ctrl Pts',(0.156449021635309,0.458528642752193,
0.0344320600360905));
#31224=CARTESIAN_POINT('Ctrl Pts',(0.168375653847077,0.470796813064372,
0.05));
#31225=CARTESIAN_POINT('Origin',(-0.0491283777357972,0.467425290823088,
0.6));
#31226=CARTESIAN_POINT('',(-0.0491283777357972,0.467425290823088,0.57));
#31227=CARTESIAN_POINT('',(-0.0668120803966779,0.495516040015929,0.54));
#31228=CARTESIAN_POINT('Ctrl Pts',(-0.0491283777357972,0.467425290823088,
0.57));
#31229=CARTESIAN_POINT('Ctrl Pts',(-0.0576967697467437,0.48103627239076,
0.555567939963917));
#31230=CARTESIAN_POINT('Ctrl Pts',(-0.0668120803966779,0.495516040015929,
0.54));
#31231=CARTESIAN_POINT('',(-0.0491283777357972,0.467425290823088,0.02));
#31232=CARTESIAN_POINT('',(-0.0491283777357972,0.467425290823088,0.6));
#31233=CARTESIAN_POINT('',(-0.0668120803966779,0.495516040015929,0.05));
#31234=CARTESIAN_POINT('Ctrl Pts',(-0.0668120803966779,0.495516040015929,
0.05));
#31235=CARTESIAN_POINT('Ctrl Pts',(-0.057696769746748,0.481036272390767,
0.0344320600360899));
#31236=CARTESIAN_POINT('Ctrl Pts',(-0.0491283777357972,0.467425290823088,
0.02));
#31237=CARTESIAN_POINT('',(-0.0668120803966779,0.495516040015929,0.295));
#31238=CARTESIAN_POINT('Origin',(-0.0226128530137678,0.539526328253384,
0.6));
#31239=CARTESIAN_POINT('',(-0.0376715015669876,0.498578838269023,0.54));
#31240=CARTESIAN_POINT('Ctrl Pts',(-0.0376715015669876,0.498578838269023,
0.54));
#31241=CARTESIAN_POINT('Ctrl Pts',(-0.0435771078395712,0.482520308657713,
0.555567939963928));
#31242=CARTESIAN_POINT('Ctrl Pts',(-0.0491283777357972,0.467425290823088,
0.57));
#31243=CARTESIAN_POINT('',(-0.0376715015669876,0.498578838269023,0.05));
#31244=CARTESIAN_POINT('',(-0.0376715015669876,0.498578838269023,0.295));
#31245=CARTESIAN_POINT('Ctrl Pts',(-0.0491283777357972,0.467425290823088,
0.02));
#31246=CARTESIAN_POINT('Ctrl Pts',(-0.0435771078395706,0.482520308657714,
0.0344320600360737));
#31247=CARTESIAN_POINT('Ctrl Pts',(-0.0376715015669877,0.498578838269023,
0.0500000000000001));
#31248=CARTESIAN_POINT('Origin',(-0.235,0.407031939778686,0.6));
#31249=CARTESIAN_POINT('',(-0.235,0.407031939778686,0.57));
#31250=CARTESIAN_POINT('',(-0.26258040326833,0.425501506248146,0.54));
#31251=CARTESIAN_POINT('Ctrl Pts',(-0.235,0.407031939778686,0.57));
#31252=CARTESIAN_POINT('Ctrl Pts',(-0.248363700552695,0.415981111160795,
0.555567939963926));
#31253=CARTESIAN_POINT('Ctrl Pts',(-0.26258040326833,0.425501506248146,
0.54));
#31254=CARTESIAN_POINT('',(-0.235,0.407031939778686,0.02));
#31255=CARTESIAN_POINT('',(-0.235,0.407031939778686,0.6));
#31256=CARTESIAN_POINT('',(-0.26258040326833,0.425501506248146,0.05));
#31257=CARTESIAN_POINT('Ctrl Pts',(-0.26258040326833,0.425501506248146,
0.05));
#31258=CARTESIAN_POINT('Ctrl Pts',(-0.248363700552693,0.415981111160794,
0.0344320600360725));
#31259=CARTESIAN_POINT('Ctrl Pts',(-0.235,0.407031939778686,0.02));
#31260=CARTESIAN_POINT('',(-0.26258040326833,0.425501506248146,0.295));
#31261=CARTESIAN_POINT('Origin',(-0.240102996759861,0.483684350529283,0.6));
#31262=CARTESIAN_POINT('',(-0.237204912125272,0.440152052890409,0.54));
#31263=CARTESIAN_POINT('Ctrl Pts',(-0.237204912125272,0.44015205289041,
0.54));
#31264=CARTESIAN_POINT('Ctrl Pts',(-0.23606835948338,0.423079829636946,
0.555567939963922));
#31265=CARTESIAN_POINT('Ctrl Pts',(-0.235,0.407031939778686,0.57));
#31266=CARTESIAN_POINT('',(-0.237204912125272,0.440152052890409,0.05));
#31267=CARTESIAN_POINT('',(-0.237204912125272,0.440152052890409,0.295));
#31268=CARTESIAN_POINT('Ctrl Pts',(-0.235,0.407031939778686,0.02));
#31269=CARTESIAN_POINT('Ctrl Pts',(-0.236068359483379,0.423079829636939,
0.034432060036071));
#31270=CARTESIAN_POINT('Ctrl Pts',(-0.237204912125272,0.440152052890409,
0.05));
#31271=CARTESIAN_POINT('Origin',(-0.380237987356225,0.276259068577462,0.6));
#31272=CARTESIAN_POINT('',(-0.380237987356225,0.276259068577462,0.57));
#31273=CARTESIAN_POINT('',(-0.412946188946813,0.281913896490228,0.54));
#31274=CARTESIAN_POINT('Ctrl Pts',(-0.380237987356225,0.276259068577462,
0.57));
#31275=CARTESIAN_POINT('Ctrl Pts',(-0.396086291219706,0.27899903674138,
0.555567939963925));
#31276=CARTESIAN_POINT('Ctrl Pts',(-0.412946188946813,0.281913896490228,
0.54));
#31277=CARTESIAN_POINT('',(-0.380237987356225,0.276259068577462,0.0200000000000001));
#31278=CARTESIAN_POINT('',(-0.380237987356225,0.276259068577462,0.6));
#31279=CARTESIAN_POINT('',(-0.412946188946813,0.281913896490228,0.05));
#31280=CARTESIAN_POINT('Ctrl Pts',(-0.412946188946813,0.281913896490228,
0.05));
#31281=CARTESIAN_POINT('Ctrl Pts',(-0.396086291219709,0.27899903674138,
0.0344320600360784));
#31282=CARTESIAN_POINT('Ctrl Pts',(-0.380237987356225,0.276259068577462,
0.0200000000000001));
#31283=CARTESIAN_POINT('',(-0.412946188946813,0.281913896490228,0.295));
#31284=CARTESIAN_POINT('Origin',(-0.416077151098926,0.344208954464292,0.6));
#31285=CARTESIAN_POINT('',(-0.395723438438122,0.305618978911176,0.54));
#31286=CARTESIAN_POINT('Ctrl Pts',(-0.395723438438122,0.305618978911176,
0.54));
#31287=CARTESIAN_POINT('Ctrl Pts',(-0.387741247158798,0.290485004512363,
0.555567939963916));
#31288=CARTESIAN_POINT('Ctrl Pts',(-0.380237987356225,0.276259068577462,
0.57));
#31289=CARTESIAN_POINT('',(-0.395723438438122,0.305618978911176,0.05));
#31290=CARTESIAN_POINT('',(-0.395723438438122,0.305618978911176,0.295));
#31291=CARTESIAN_POINT('Ctrl Pts',(-0.380237987356225,0.276259068577462,
0.0200000000000001));
#31292=CARTESIAN_POINT('Ctrl Pts',(-0.387741247158788,0.290485004512343,
0.0344320600360639));
#31293=CARTESIAN_POINT('Ctrl Pts',(-0.395723438438122,0.305618978911176,
0.05));
#31294=CARTESIAN_POINT('Origin',(-0.459729372344889,0.0977184946843469,
0.6));
#31295=CARTESIAN_POINT('',(-0.459729372344889,0.0977184946843469,0.57));
#31296=CARTESIAN_POINT('',(-0.491909827058038,0.0895808129218024,0.54));
#31297=CARTESIAN_POINT('Ctrl Pts',(-0.459729372344889,0.0977184946843469,
0.57));
#31298=CARTESIAN_POINT('Ctrl Pts',(-0.47532196380384,0.0937754942427011,
0.555567939963923));
#31299=CARTESIAN_POINT('Ctrl Pts',(-0.491909827058038,0.0895808129218025,
0.54));
#31300=CARTESIAN_POINT('',(-0.459729372344889,0.0977184946843469,0.0200000000000001));
#31301=CARTESIAN_POINT('',(-0.459729372344889,0.0977184946843469,0.6));
#31302=CARTESIAN_POINT('',(-0.491909827058038,0.0895808129218024,0.05));
#31303=CARTESIAN_POINT('Ctrl Pts',(-0.491909827058038,0.0895808129218025,
0.05));
#31304=CARTESIAN_POINT('Ctrl Pts',(-0.47532196380385,0.0937754942426984,
0.0344320600360872));
#31305=CARTESIAN_POINT('Ctrl Pts',(-0.459729372344889,0.0977184946843469,
0.0200000000000001));
#31306=CARTESIAN_POINT('',(-0.491909827058038,0.0895808129218024,0.295));
#31307=CARTESIAN_POINT('Origin',(-0.520107786070735,0.145216703132244,0.6));
#31308=CARTESIAN_POINT('',(-0.485817787210443,0.11824160701694,0.54));
#31309=CARTESIAN_POINT('Ctrl Pts',(-0.485817787210443,0.11824160701694,
0.54));
#31310=CARTESIAN_POINT('Ctrl Pts',(-0.47237015068181,0.107662683134162,
0.555567939963921));
#31311=CARTESIAN_POINT('Ctrl Pts',(-0.459729372344889,0.0977184946843469,
0.57));
#31312=CARTESIAN_POINT('',(-0.485817787210443,0.11824160701694,0.05));
#31313=CARTESIAN_POINT('',(-0.485817787210443,0.11824160701694,0.295));
#31314=CARTESIAN_POINT('Ctrl Pts',(-0.459729372344889,0.0977184946843469,
0.0200000000000001));
#31315=CARTESIAN_POINT('Ctrl Pts',(-0.472370150681809,0.107662683134161,
0.0344320600360776));
#31316=CARTESIAN_POINT('Ctrl Pts',(-0.485817787210443,0.11824160701694,
0.05));
#31317=CARTESIAN_POINT('Origin',(-0.47,5.75583995599256E-17,0.6));
#31318=CARTESIAN_POINT('',(-0.47,5.75583995599256E-17,0.57));
#31319=CARTESIAN_POINT('',(-0.499785315393603,-0.0146505466422634,0.54));
#31320=CARTESIAN_POINT('Ctrl Pts',(-0.47,5.75583995599256E-17,0.57));
#31321=CARTESIAN_POINT('Ctrl Pts',(-0.484432060036081,-0.0070987184761509,
0.555567939963919));
#31322=CARTESIAN_POINT('Ctrl Pts',(-0.499785315393603,-0.0146505466422634,
0.54));
#31323=CARTESIAN_POINT('',(-0.47,5.75583995599256E-17,0.0200000000000001));
#31324=CARTESIAN_POINT('',(-0.47,5.75583995599256E-17,0.6));
#31325=CARTESIAN_POINT('',(-0.499785315393603,-0.0146505466422634,0.05));
#31326=CARTESIAN_POINT('Ctrl Pts',(-0.499785315393603,-0.0146505466422634,
0.05));
#31327=CARTESIAN_POINT('Ctrl Pts',(-0.484432060036073,-0.00709871847614705,
0.0344320600360732));
#31328=CARTESIAN_POINT('Ctrl Pts',(-0.47,5.75583995599256E-17,0.0200000000000001));
#31329=CARTESIAN_POINT('',(-0.499785315393603,-0.0146505466422634,0.295));
#31330=CARTESIAN_POINT('Origin',(-0.538934433351267,0.0339068805458291,
0.6));
#31331=CARTESIAN_POINT('',(-0.499785315393603,0.0146505466422634,0.54));
#31332=CARTESIAN_POINT('Ctrl Pts',(-0.499785315393603,0.0146505466422635,
0.54));
#31333=CARTESIAN_POINT('Ctrl Pts',(-0.48443206003608,0.00709871847615045,
0.55556793996392));
#31334=CARTESIAN_POINT('Ctrl Pts',(-0.47,5.75583995599256E-17,0.57));
#31335=CARTESIAN_POINT('',(-0.499785315393603,0.0146505466422634,0.05));
#31336=CARTESIAN_POINT('',(-0.499785315393603,0.0146505466422634,0.295));
#31337=CARTESIAN_POINT('Ctrl Pts',(-0.47,5.75583995599256E-17,0.0200000000000001));
#31338=CARTESIAN_POINT('Ctrl Pts',(-0.484432060036083,0.007098718476152,
0.0344320600360831));
#31339=CARTESIAN_POINT('Ctrl Pts',(-0.499785315393603,0.0146505466422634,
0.05));
#31340=CARTESIAN_POINT('Origin',(-0.429366365092022,-0.191166222245626,
0.6));
#31341=CARTESIAN_POINT('',(-0.429366365092022,-0.191166222245626,0.57));
#31342=CARTESIAN_POINT('',(-0.450617690513801,-0.216664941778795,0.54));
#31343=CARTESIAN_POINT('Ctrl Pts',(-0.429366365092022,-0.191166222245626,
0.57));
#31344=CARTESIAN_POINT('Ctrl Pts',(-0.439663399059279,-0.20352127191634,
0.55556793996392));
#31345=CARTESIAN_POINT('Ctrl Pts',(-0.450617690513801,-0.216664941778795,
0.54));
#31346=CARTESIAN_POINT('',(-0.429366365092022,-0.191166222245626,0.02));
#31347=CARTESIAN_POINT('',(-0.429366365092022,-0.191166222245626,0.6));
#31348=CARTESIAN_POINT('',(-0.450617690513801,-0.216664941778795,0.05));
#31349=CARTESIAN_POINT('Ctrl Pts',(-0.450617690513801,-0.216664941778795,
0.05));
#31350=CARTESIAN_POINT('Ctrl Pts',(-0.439663399059269,-0.203521271916329,
0.0344320600360665));
#31351=CARTESIAN_POINT('Ctrl Pts',(-0.429366365092022,-0.191166222245626,
0.02));
#31352=CARTESIAN_POINT('',(-0.450617690513801,-0.216664941778795,0.295));
#31353=CARTESIAN_POINT('Origin',(-0.506132274325621,-0.18822890555378,0.6));
#31354=CARTESIAN_POINT('',(-0.4625355188348,-0.189897061104753,0.54));
#31355=CARTESIAN_POINT('Ctrl Pts',(-0.4625355188348,-0.189897061104753,
0.54));
#31356=CARTESIAN_POINT('Ctrl Pts',(-0.445438016905532,-0.190551267878399,
0.555567939963925));
#31357=CARTESIAN_POINT('Ctrl Pts',(-0.429366365092022,-0.191166222245626,
0.57));
#31358=CARTESIAN_POINT('',(-0.4625355188348,-0.189897061104753,0.05));
#31359=CARTESIAN_POINT('',(-0.4625355188348,-0.189897061104753,0.295));
#31360=CARTESIAN_POINT('Ctrl Pts',(-0.429366365092022,-0.191166222245626,
0.02));
#31361=CARTESIAN_POINT('Ctrl Pts',(-0.445438016905514,-0.1905512678784,
0.0344320600360582));
#31362=CARTESIAN_POINT('Ctrl Pts',(-0.4625355188348,-0.189897061104753,
0.05));
#31363=CARTESIAN_POINT('Origin',(-0.314491384988663,-0.349278067974375,
0.6));
#31364=CARTESIAN_POINT('',(-0.314491384988663,-0.349278067974375,0.57));
#31365=CARTESIAN_POINT('',(-0.323534173210961,-0.38121600014257,0.54));
#31366=CARTESIAN_POINT('Ctrl Pts',(-0.314491384988663,-0.349278067974375,
0.57));
#31367=CARTESIAN_POINT('Ctrl Pts',(-0.318872942168543,-0.364753148509492,
0.555567939963913));
#31368=CARTESIAN_POINT('Ctrl Pts',(-0.323534173210961,-0.38121600014257,
0.54));
#31369=CARTESIAN_POINT('',(-0.314491384988663,-0.349278067974375,0.0200000000000001));
#31370=CARTESIAN_POINT('',(-0.314491384988663,-0.349278067974375,0.6));
#31371=CARTESIAN_POINT('',(-0.323534173210961,-0.38121600014257,0.05));
#31372=CARTESIAN_POINT('Ctrl Pts',(-0.323534173210961,-0.38121600014257,
0.05));
#31373=CARTESIAN_POINT('Ctrl Pts',(-0.318872942168548,-0.364753148509509,
0.0344320600361024));
#31374=CARTESIAN_POINT('Ctrl Pts',(-0.314491384988663,-0.349278067974375,
0.0200000000000001));
#31375=CARTESIAN_POINT('',(-0.323534173210961,-0.38121600014257,0.295));
#31376=CARTESIAN_POINT('Origin',(-0.385815247001714,-0.377818203877217,
0.6));
#31377=CARTESIAN_POINT('',(-0.345309129066188,-0.361609741826117,0.54));
#31378=CARTESIAN_POINT('Ctrl Pts',(-0.345309129066188,-0.361609741826117,
0.54));
#31379=CARTESIAN_POINT('Ctrl Pts',(-0.32942369397469,-0.355253208912852,
0.555567939963916));
#31380=CARTESIAN_POINT('Ctrl Pts',(-0.314491384988663,-0.349278067974375,
0.57));
#31381=CARTESIAN_POINT('',(-0.345309129066188,-0.361609741826117,0.05));
#31382=CARTESIAN_POINT('',(-0.345309129066188,-0.361609741826117,0.295));
#31383=CARTESIAN_POINT('Ctrl Pts',(-0.314491384988663,-0.349278067974375,
0.0200000000000001));
#31384=CARTESIAN_POINT('Ctrl Pts',(-0.329423693974684,-0.355253208912849,
0.0344320600360788));
#31385=CARTESIAN_POINT('Ctrl Pts',(-0.345309129066188,-0.361609741826117,
0.0500000000000001));
#31386=CARTESIAN_POINT('Origin',(-0.145237987356225,-0.446996562658722,
0.6));
#31387=CARTESIAN_POINT('',(-0.145237987356225,-0.446996562658722,0.57));
#31388=CARTESIAN_POINT('',(-0.140508658144256,-0.479851348843057,0.54));
#31389=CARTESIAN_POINT('Ctrl Pts',(-0.145237987356225,-0.446996562658722,
0.57));
#31390=CARTESIAN_POINT('Ctrl Pts',(-0.142946456707126,-0.462915892047014,
0.555567939963919));
#31391=CARTESIAN_POINT('Ctrl Pts',(-0.140508658144256,-0.479851348843057,
0.54));
#31392=CARTESIAN_POINT('',(-0.145237987356225,-0.446996562658722,0.02));
#31393=CARTESIAN_POINT('',(-0.145237987356225,-0.446996562658722,0.6));
#31394=CARTESIAN_POINT('',(-0.140508658144256,-0.479851348843057,0.05));
#31395=CARTESIAN_POINT('Ctrl Pts',(-0.140508658144256,-0.479851348843057,
0.05));
#31396=CARTESIAN_POINT('Ctrl Pts',(-0.142946456707126,-0.462915892047012,
0.0344320600360792));
#31397=CARTESIAN_POINT('Ctrl Pts',(-0.145237987356225,-0.446996562658722,
0.02));
#31398=CARTESIAN_POINT('',(-0.140508658144256,-0.479851348843057,0.295));
#31399=CARTESIAN_POINT('Origin',(-0.198787258449726,-0.502079302379656,
0.6));
#31400=CARTESIAN_POINT('',(-0.168375653847077,-0.470796813064372,0.54));
#31401=CARTESIAN_POINT('Ctrl Pts',(-0.168375653847077,-0.470796813064372,
0.54));
#31402=CARTESIAN_POINT('Ctrl Pts',(-0.156449021635299,-0.458528642752182,
0.555567939963923));
#31403=CARTESIAN_POINT('Ctrl Pts',(-0.145237987356225,-0.446996562658722,
0.57));
#31404=CARTESIAN_POINT('',(-0.168375653847077,-0.470796813064372,0.05));
#31405=CARTESIAN_POINT('',(-0.168375653847077,-0.470796813064372,0.295));
#31406=CARTESIAN_POINT('Ctrl Pts',(-0.145237987356225,-0.446996562658722,
0.02));
#31407=CARTESIAN_POINT('Ctrl Pts',(-0.156449021635308,-0.458528642752192,
0.0344320600360887));
#31408=CARTESIAN_POINT('Ctrl Pts',(-0.168375653847077,-0.470796813064372,
0.05));
#31409=CARTESIAN_POINT('Origin',(0.0491283777357969,-0.467425290823089,
0.6));
#31410=CARTESIAN_POINT('',(0.0491283777357969,-0.467425290823089,0.57));
#31411=CARTESIAN_POINT('',(0.0668120803966778,-0.495516040015929,0.54));
#31412=CARTESIAN_POINT('Ctrl Pts',(0.0491283777357969,-0.467425290823089,
0.57));
#31413=CARTESIAN_POINT('Ctrl Pts',(0.0576967697467424,-0.481036272390759,
0.555567939963919));
#31414=CARTESIAN_POINT('Ctrl Pts',(0.0668120803966778,-0.495516040015929,
0.54));
#31415=CARTESIAN_POINT('',(0.0491283777357969,-0.467425290823089,0.0200000000000001));
#31416=CARTESIAN_POINT('',(0.0491283777357969,-0.467425290823089,0.6));
#31417=CARTESIAN_POINT('',(0.0668120803966778,-0.495516040015929,0.05));
#31418=CARTESIAN_POINT('Ctrl Pts',(0.0668120803966778,-0.495516040015929,
0.05));
#31419=CARTESIAN_POINT('Ctrl Pts',(0.0576967697467371,-0.48103627239075,
0.0344320600360721));
#31420=CARTESIAN_POINT('Ctrl Pts',(0.0491283777357969,-0.467425290823089,
0.0200000000000001));
#31421=CARTESIAN_POINT('',(0.0668120803966778,-0.495516040015929,0.295));
#31422=CARTESIAN_POINT('Origin',(0.0226128530137677,-0.539526328253384,
0.6));
#31423=CARTESIAN_POINT('',(0.0376715015669875,-0.498578838269023,0.54));
#31424=CARTESIAN_POINT('Ctrl Pts',(0.0376715015669875,-0.498578838269023,
0.54));
#31425=CARTESIAN_POINT('Ctrl Pts',(0.0435771078395709,-0.482520308657713,
0.555567939963928));
#31426=CARTESIAN_POINT('Ctrl Pts',(0.0491283777357969,-0.467425290823089,
0.57));
#31427=CARTESIAN_POINT('',(0.0376715015669875,-0.498578838269023,0.05));
#31428=CARTESIAN_POINT('',(0.0376715015669875,-0.498578838269023,0.295));
#31429=CARTESIAN_POINT('Ctrl Pts',(0.0491283777357969,-0.467425290823089,
0.0200000000000001));
#31430=CARTESIAN_POINT('Ctrl Pts',(0.0435771078395724,-0.482520308657709,
0.0344320600360687));
#31431=CARTESIAN_POINT('Ctrl Pts',(0.0376715015669875,-0.498578838269023,
0.0500000000000001));
#31432=CARTESIAN_POINT('Origin',(0.235,-0.407031939778686,0.6));
#31433=CARTESIAN_POINT('',(0.235,-0.407031939778686,0.57));
#31434=CARTESIAN_POINT('',(0.26258040326833,-0.425501506248146,0.54));
#31435=CARTESIAN_POINT('Ctrl Pts',(0.235,-0.407031939778686,0.57));
#31436=CARTESIAN_POINT('Ctrl Pts',(0.2483637005527,-0.415981111160798,0.555567939963921));
#31437=CARTESIAN_POINT('Ctrl Pts',(0.26258040326833,-0.425501506248146,
0.54));
#31438=CARTESIAN_POINT('',(0.235,-0.407031939778686,0.0200000000000001));
#31439=CARTESIAN_POINT('',(0.235,-0.407031939778686,0.6));
#31440=CARTESIAN_POINT('',(0.26258040326833,-0.425501506248146,0.05));
#31441=CARTESIAN_POINT('Ctrl Pts',(0.26258040326833,-0.425501506248146,
0.05));
#31442=CARTESIAN_POINT('Ctrl Pts',(0.248363700552693,-0.415981111160793,
0.0344320600360718));
#31443=CARTESIAN_POINT('Ctrl Pts',(0.235,-0.407031939778686,0.0200000000000001));
#31444=CARTESIAN_POINT('',(0.26258040326833,-0.425501506248146,0.295));
#31445=CARTESIAN_POINT('Origin',(0.240102996759861,-0.483684350529283,0.6));
#31446=CARTESIAN_POINT('',(0.237204912125272,-0.440152052890409,0.54));
#31447=CARTESIAN_POINT('Ctrl Pts',(0.237204912125272,-0.44015205289041,
0.54));
#31448=CARTESIAN_POINT('Ctrl Pts',(0.23606835948338,-0.423079829636952,
0.555567939963918));
#31449=CARTESIAN_POINT('Ctrl Pts',(0.235,-0.407031939778686,0.57));
#31450=CARTESIAN_POINT('',(0.237204912125272,-0.440152052890409,0.05));
#31451=CARTESIAN_POINT('',(0.237204912125272,-0.440152052890409,0.295));
#31452=CARTESIAN_POINT('Ctrl Pts',(0.235,-0.407031939778686,0.0200000000000001));
#31453=CARTESIAN_POINT('Ctrl Pts',(0.236068359483379,-0.423079829636935,
0.0344320600360673));
#31454=CARTESIAN_POINT('Ctrl Pts',(0.237204912125272,-0.440152052890409,
0.05));
#31455=CARTESIAN_POINT('Origin',(0.380237987356225,-0.276259068577463,0.6));
#31456=CARTESIAN_POINT('',(0.380237987356225,-0.276259068577463,0.57));
#31457=CARTESIAN_POINT('',(0.412946188946813,-0.281913896490228,0.54));
#31458=CARTESIAN_POINT('Ctrl Pts',(0.380237987356225,-0.276259068577463,
0.57));
#31459=CARTESIAN_POINT('Ctrl Pts',(0.3960862912197,-0.278999036741379,0.55556793996393));
#31460=CARTESIAN_POINT('Ctrl Pts',(0.412946188946813,-0.281913896490228,
0.54));
#31461=CARTESIAN_POINT('',(0.380237987356225,-0.276259068577462,0.0200000000000001));
#31462=CARTESIAN_POINT('',(0.380237987356225,-0.276259068577463,0.6));
#31463=CARTESIAN_POINT('',(0.412946188946813,-0.281913896490228,0.05));
#31464=CARTESIAN_POINT('Ctrl Pts',(0.412946188946813,-0.281913896490228,
0.05));
#31465=CARTESIAN_POINT('Ctrl Pts',(0.396086291219706,-0.27899903674138,
0.0344320600360757));
#31466=CARTESIAN_POINT('Ctrl Pts',(0.380237987356225,-0.276259068577462,
0.0200000000000001));
#31467=CARTESIAN_POINT('',(0.412946188946813,-0.281913896490228,0.295));
#31468=CARTESIAN_POINT('Origin',(0.416077151098926,-0.344208954464293,0.6));
#31469=CARTESIAN_POINT('',(0.395723438438122,-0.305618978911176,0.54));
#31470=CARTESIAN_POINT('Ctrl Pts',(0.395723438438122,-0.305618978911176,
0.54));
#31471=CARTESIAN_POINT('Ctrl Pts',(0.387741247158795,-0.290485004512358,
0.555567939963921));
#31472=CARTESIAN_POINT('Ctrl Pts',(0.380237987356225,-0.276259068577463,
0.57));
#31473=CARTESIAN_POINT('',(0.395723438438122,-0.305618978911176,0.05));
#31474=CARTESIAN_POINT('',(0.395723438438122,-0.305618978911176,0.295));
#31475=CARTESIAN_POINT('Ctrl Pts',(0.380237987356225,-0.276259068577462,
0.0200000000000001));
#31476=CARTESIAN_POINT('Ctrl Pts',(0.387741247158799,-0.290485004512365,
0.0344320600360857));
#31477=CARTESIAN_POINT('Ctrl Pts',(0.395723438438122,-0.305618978911176,
0.05));
#31478=CARTESIAN_POINT('Origin',(0.459729372344889,-0.0977184946843472,
0.6));
#31479=CARTESIAN_POINT('',(0.459729372344889,-0.0977184946843472,0.57));
#31480=CARTESIAN_POINT('',(0.491909827058038,-0.0895808129218025,0.54));
#31481=CARTESIAN_POINT('Ctrl Pts',(0.459729372344889,-0.0977184946843472,
0.57));
#31482=CARTESIAN_POINT('Ctrl Pts',(0.475321963803834,-0.0937754942427026,
0.555567939963928));
#31483=CARTESIAN_POINT('Ctrl Pts',(0.491909827058038,-0.0895808129218025,
0.54));
#31484=CARTESIAN_POINT('',(0.459729372344889,-0.0977184946843472,0.0200000000000001));
#31485=CARTESIAN_POINT('',(0.459729372344889,-0.0977184946843472,0.6));
#31486=CARTESIAN_POINT('',(0.491909827058038,-0.0895808129218025,0.05));
#31487=CARTESIAN_POINT('Ctrl Pts',(0.491909827058038,-0.0895808129218025,
0.05));
#31488=CARTESIAN_POINT('Ctrl Pts',(0.475321963803832,-0.0937754942427031,
0.034432060036071));
#31489=CARTESIAN_POINT('Ctrl Pts',(0.459729372344889,-0.0977184946843472,
0.0200000000000001));
#31490=CARTESIAN_POINT('',(0.491909827058038,-0.0895808129218025,0.295));
#31491=CARTESIAN_POINT('Origin',(0.520107786070735,-0.145216703132244,0.6));
#31492=CARTESIAN_POINT('',(0.485817787210443,-0.11824160701694,0.54));
#31493=CARTESIAN_POINT('Ctrl Pts',(0.485817787210443,-0.11824160701694,
0.54));
#31494=CARTESIAN_POINT('Ctrl Pts',(0.472370150681812,-0.107662683134164,
0.555567939963919));
#31495=CARTESIAN_POINT('Ctrl Pts',(0.459729372344889,-0.0977184946843472,
0.57));
#31496=CARTESIAN_POINT('',(0.485817787210443,-0.11824160701694,0.05));
#31497=CARTESIAN_POINT('',(0.485817787210443,-0.11824160701694,0.295));
#31498=CARTESIAN_POINT('Ctrl Pts',(0.459729372344889,-0.0977184946843472,
0.0200000000000001));
#31499=CARTESIAN_POINT('Ctrl Pts',(0.4723701506818,-0.107662683134155,0.0344320600360681));
#31500=CARTESIAN_POINT('Ctrl Pts',(0.485817787210443,-0.11824160701694,
0.05));
#31501=CARTESIAN_POINT('Origin',(0.,0.,0.295));
#31502=CARTESIAN_POINT('Origin',(0.,0.,0.05));
#31503=CARTESIAN_POINT('Origin',(0.,0.,0.54));
#31504=CARTESIAN_POINT('Origin',(0.,0.,0.295));
#31505=CARTESIAN_POINT('Origin',(0.,0.,0.05));
#31506=CARTESIAN_POINT('Origin',(0.,0.,0.54));
#31507=CARTESIAN_POINT('Origin',(0.,0.,0.295));
#31508=CARTESIAN_POINT('Origin',(0.,0.,0.54));
#31509=CARTESIAN_POINT('Origin',(0.,0.,0.05));
#31510=CARTESIAN_POINT('Origin',(0.,0.,0.295));
#31511=CARTESIAN_POINT('Origin',(0.,0.,0.05));
#31512=CARTESIAN_POINT('Origin',(0.,0.,0.54));
#31513=CARTESIAN_POINT('Origin',(0.,0.,0.295));
#31514=CARTESIAN_POINT('Origin',(0.,0.,0.54));
#31515=CARTESIAN_POINT('Origin',(0.,0.,0.05));
#31516=CARTESIAN_POINT('Origin',(0.,0.,0.295));
#31517=CARTESIAN_POINT('Origin',(0.,0.,0.05));
#31518=CARTESIAN_POINT('Origin',(0.,0.,0.54));
#31519=CARTESIAN_POINT('Origin',(0.,0.,0.295));
#31520=CARTESIAN_POINT('Origin',(0.,0.,0.54));
#31521=CARTESIAN_POINT('Origin',(0.,0.,0.05));
#31522=CARTESIAN_POINT('Origin',(0.,0.,0.295));
#31523=CARTESIAN_POINT('Origin',(0.,0.,0.05));
#31524=CARTESIAN_POINT('Origin',(0.,0.,0.54));
#31525=CARTESIAN_POINT('Origin',(0.,0.,0.295));
#31526=CARTESIAN_POINT('Origin',(0.,0.,0.54));
#31527=CARTESIAN_POINT('Origin',(0.,0.,0.05));
#31528=CARTESIAN_POINT('Origin',(0.,0.,0.295));
#31529=CARTESIAN_POINT('Origin',(0.,0.,0.05));
#31530=CARTESIAN_POINT('Origin',(0.,0.,0.54));
#31531=CARTESIAN_POINT('Origin',(0.,0.,0.295));
#31532=CARTESIAN_POINT('Origin',(0.,0.,0.54));
#31533=CARTESIAN_POINT('Origin',(0.,0.,0.05));
#31534=CARTESIAN_POINT('Origin',(0.,0.,0.295));
#31535=CARTESIAN_POINT('Origin',(0.,0.,0.05));
#31536=CARTESIAN_POINT('Origin',(0.,0.,0.54));
#31537=CARTESIAN_POINT('Origin',(0.,0.,0.295));
#31538=CARTESIAN_POINT('Origin',(0.,0.,0.54));
#31539=CARTESIAN_POINT('Origin',(0.,0.,0.05));
#31540=CARTESIAN_POINT('Origin',(0.,0.,0.295));
#31541=CARTESIAN_POINT('Origin',(0.,0.,0.05));
#31542=CARTESIAN_POINT('Origin',(0.,0.,0.54));
#31543=CARTESIAN_POINT('Origin',(0.,0.,0.295));
#31544=CARTESIAN_POINT('Origin',(0.,0.,0.54));
#31545=CARTESIAN_POINT('Origin',(0.,0.,0.05));
#31546=CARTESIAN_POINT('Origin',(0.,0.,0.295));
#31547=CARTESIAN_POINT('Origin',(0.,0.,0.05));
#31548=CARTESIAN_POINT('Origin',(0.,0.,0.54));
#31549=CARTESIAN_POINT('Origin',(0.,0.,0.295));
#31550=CARTESIAN_POINT('Origin',(0.,0.,0.54));
#31551=CARTESIAN_POINT('Origin',(0.,0.,0.05));
#31552=CARTESIAN_POINT('Origin',(0.,0.,0.295));
#31553=CARTESIAN_POINT('Origin',(0.,0.,0.05));
#31554=CARTESIAN_POINT('Origin',(0.,0.,0.54));
#31555=CARTESIAN_POINT('Origin',(0.,0.,0.295));
#31556=CARTESIAN_POINT('Origin',(0.,0.,0.54));
#31557=CARTESIAN_POINT('Origin',(0.,0.,0.05));
#31558=CARTESIAN_POINT('Origin',(0.,0.,0.295));
#31559=CARTESIAN_POINT('Origin',(0.,0.,0.05));
#31560=CARTESIAN_POINT('Origin',(0.,0.,0.54));
#31561=CARTESIAN_POINT('Origin',(0.,0.,0.295));
#31562=CARTESIAN_POINT('Origin',(0.,0.,0.54));
#31563=CARTESIAN_POINT('Origin',(0.,0.,0.05));
#31564=CARTESIAN_POINT('Origin',(0.,0.,0.295));
#31565=CARTESIAN_POINT('Origin',(0.,0.,0.05));
#31566=CARTESIAN_POINT('Origin',(0.,0.,0.54));
#31567=CARTESIAN_POINT('Origin',(0.,0.,0.295));
#31568=CARTESIAN_POINT('Origin',(0.,0.,0.54));
#31569=CARTESIAN_POINT('Origin',(0.,0.,0.05));
#31570=CARTESIAN_POINT('Origin',(0.,0.,0.295));
#31571=CARTESIAN_POINT('Origin',(0.,0.,0.05));
#31572=CARTESIAN_POINT('Origin',(0.,0.,0.54));
#31573=CARTESIAN_POINT('Origin',(0.,0.,0.295));
#31574=CARTESIAN_POINT('Origin',(0.,0.,0.54));
#31575=CARTESIAN_POINT('Origin',(0.,0.,0.05));
#31576=CARTESIAN_POINT('Origin',(0.,0.,0.295));
#31577=CARTESIAN_POINT('Origin',(0.,0.,0.05));
#31578=CARTESIAN_POINT('Origin',(0.,0.,0.54));
#31579=CARTESIAN_POINT('Origin',(0.,0.,0.295));
#31580=CARTESIAN_POINT('Origin',(0.,0.,0.54));
#31581=CARTESIAN_POINT('Origin',(0.,0.,0.05));
#31582=CARTESIAN_POINT('Origin',(0.,0.,0.295));
#31583=CARTESIAN_POINT('Origin',(0.,0.,0.05));
#31584=CARTESIAN_POINT('Origin',(0.,0.,0.54));
#31585=CARTESIAN_POINT('Origin',(0.,0.,0.295));
#31586=CARTESIAN_POINT('Origin',(0.,0.,0.54));
#31587=CARTESIAN_POINT('Origin',(0.,0.,0.05));
#31588=CARTESIAN_POINT('Origin',(0.,0.,0.295));
#31589=CARTESIAN_POINT('Origin',(0.,0.,0.05));
#31590=CARTESIAN_POINT('Origin',(0.,0.,0.54));
#31591=CARTESIAN_POINT('Origin',(0.,0.,0.025));
#31592=CARTESIAN_POINT('',(-0.45,-5.51091059616309E-17,2.42861286636753E-17));
#31593=CARTESIAN_POINT('',(-0.475,-5.81707229594993E-17,0.025));
#31594=CARTESIAN_POINT('Origin',(0.,0.,0.));
#31595=CARTESIAN_POINT('Origin',(0.21,0.,-1.2));
#31596=CARTESIAN_POINT('',(-0.21,-2.57175827820944E-17,-1.2));
#31597=CARTESIAN_POINT('Origin',(0.,0.,-1.2));
#31598=CARTESIAN_POINT('Origin',(0.,0.,-1.18));
#31599=CARTESIAN_POINT('',(-0.23,-2.81668763803891E-17,-1.18));
#31600=CARTESIAN_POINT('Origin',(0.,0.,-0.58));
#31601=CARTESIAN_POINT('Origin',(0.,0.,0.));
#31602=CARTESIAN_POINT('Origin',(0.45,0.,0.));
#31603=CARTESIAN_POINT('Origin',(0.,0.,0.57));
#31604=CARTESIAN_POINT('',(-0.44,-5.38844591624836E-17,0.6));
#31605=CARTESIAN_POINT('Origin',(0.,0.,0.6));
#31606=CARTESIAN_POINT('',(-0.47,-5.75583995599256E-17,0.57));
#31607=CARTESIAN_POINT('Origin',(0.,0.,0.6));
#31608=CARTESIAN_POINT('',(0.,0.,0.));
#31609=CARTESIAN_POINT('Origin',(0.,0.,0.));
#31610=CARTESIAN_POINT('',(-9.18485099360515E-18,-1.12481983699639E-33,
0.15));
#31611=CARTESIAN_POINT('',(-9.18485099360515E-18,-1.12481983699639E-33,
-0.15));
#31612=CARTESIAN_POINT('Origin',(0.,0.,0.));
#31613=CARTESIAN_POINT('',(0.,0.,0.));
#31614=CARTESIAN_POINT('Ctrl Pts',(0.329995701589468,0.00118959959741402,
0.00102359537366932));
#31615=CARTESIAN_POINT('Ctrl Pts',(0.329812358348379,0.0519304593106012,
0.00303724894968045));
#31616=CARTESIAN_POINT('Ctrl Pts',(0.307603150250096,0.14856309907024,0.007063921474547));
#31617=CARTESIAN_POINT('Ctrl Pts',(0.212522007054295,0.2688270154723,0.0131144005095069));
#31618=CARTESIAN_POINT('Ctrl Pts',(0.0751961041762406,0.33443845631537,
0.0191752186885983));
#31619=CARTESIAN_POINT('Ctrl Pts',(-0.0776142387319525,0.334810528053721,
0.025245738062024));
#31620=CARTESIAN_POINT('Ctrl Pts',(-0.215432226705683,0.268236493442132,
0.0313264548832147));
#31621=CARTESIAN_POINT('Ctrl Pts',(-0.311063582237146,0.148538498980413,
0.0374170400486292));
#31622=CARTESIAN_POINT('Ctrl Pts',(-0.339534702539374,0.0237758430999062,
0.0425008539245673));
#31623=CARTESIAN_POINT('Ctrl Pts',(-0.329617478537296,-0.0636510452603832,
0.0460638560210726));
#31624=CARTESIAN_POINT('Ctrl Pts',(-0.315752180564557,-0.111758567679568,
0.0481010960909614));
#31625=CARTESIAN_POINT('Ctrl Pts',(-0.280687728436729,-0.19663499457563,
0.0518375549362775));
#31626=CARTESIAN_POINT('Ctrl Pts',(-0.176953832876605,-0.308707864139412,
0.0577895429568186));
#31627=CARTESIAN_POINT('Ctrl Pts',(0.0277912542949835,-0.355359243876355,
0.0659698006169508));
#31628=CARTESIAN_POINT('Ctrl Pts',(0.207256209567046,-0.285022432777545,
0.073484386523706));
#31629=CARTESIAN_POINT('Ctrl Pts',(0.31450859302708,-0.150158997366471,
0.0803284879538114));
#31630=CARTESIAN_POINT('Ctrl Pts',(0.349186611535958,0.00111014849211965,
0.0864979120385476));
#31631=CARTESIAN_POINT('Ctrl Pts',(0.314520756767304,0.152731777144028,
0.0926770234710082));
#31632=CARTESIAN_POINT('Ctrl Pts',(0.217500483746742,0.274539465175591,
0.098865768103921));
#31633=CARTESIAN_POINT('Ctrl Pts',(0.0769551264679099,0.342186713109751,
0.105064101576398));
#31634=CARTESIAN_POINT('Ctrl Pts',(-0.0793009475509065,0.342263708237282,
0.111271969453101));
#31635=CARTESIAN_POINT('Ctrl Pts',(-0.220172034550062,0.274381760656883,
0.117489309777858));
#31636=CARTESIAN_POINT('Ctrl Pts',(-0.318128621603507,0.151819046241454,
0.123716067105663));
#31637=CARTESIAN_POINT('Ctrl Pts',(-0.352617648223723,-0.000927697002303161,
0.129952164368648));
#31638=CARTESIAN_POINT('Ctrl Pts',(-0.307197248189229,-0.205991895653557,
0.138279361997572));
#31639=CARTESIAN_POINT('Ctrl Pts',(-0.0867093646975666,-0.382606488631909,
0.148711360096893));
#31640=CARTESIAN_POINT('Ctrl Pts',(0.246157896760925,-0.307226237821677,
0.16126605881999));
#31641=CARTESIAN_POINT('Ctrl Pts',(0.394548713993526,0.00121213976701099,
0.173856329664019));
#31642=CARTESIAN_POINT('Ctrl Pts',(0.270683494680064,0.25779707362797,0.184377360469391));
#31643=CARTESIAN_POINT('Ctrl Pts',(0.0784480660104459,0.348945360245205,
0.192811248605432));
#31644=CARTESIAN_POINT('Ctrl Pts',(-0.0805931042682236,0.349358375490888,
0.199145126960344));
#31645=CARTESIAN_POINT('Ctrl Pts',(-0.224524686851408,0.279914574363962,
0.205487348255157));
#31646=CARTESIAN_POINT('Ctrl Pts',(-0.324178791380424,0.155094279198964,
0.211837815149481));
#31647=CARTESIAN_POINT('Ctrl Pts',(-0.359765231562575,-0.000950160030172512,
0.218196411362682));
#31648=CARTESIAN_POINT('Ctrl Pts',(-0.324199918380757,-0.157162565812712,
0.22456305908972));
#31649=CARTESIAN_POINT('Ctrl Pts',(-0.224151419632265,-0.282543079616346,
0.230937631934188));
#31650=CARTESIAN_POINT('Ctrl Pts',(-0.0794762745603369,-0.352337612459348,
0.237319995378052));
#31651=CARTESIAN_POINT('Ctrl Pts',(0.0812906306420514,-0.352242766117238,
0.243710053380832));
#31652=CARTESIAN_POINT('Ctrl Pts',(0.242583044989387,-0.274824345329341,
0.250818566710242));
#31653=CARTESIAN_POINT('Ctrl Pts',(0.355857692111688,-0.108936398125315,
0.258648506513342));
#31654=CARTESIAN_POINT('Ctrl Pts',(0.35601905515454,0.110643209305051,0.267203260973594));
#31655=CARTESIAN_POINT('Ctrl Pts',(0.232065828412221,0.292295611594562,
0.275770669585301));
#31656=CARTESIAN_POINT('Ctrl Pts',(0.0272435837717024,0.37290401539681,
0.284350408116761));
#31657=CARTESIAN_POINT('Ctrl Pts',(-0.187879927304316,0.323810447294939,
0.292942183858905));
#31658=CARTESIAN_POINT('Ctrl Pts',(-0.325407735789747,0.17542191209667,
0.300828814614272));
#31659=CARTESIAN_POINT('Ctrl Pts',(-0.365431318619722,-0.00075089577638709,
0.308006589851792));
#31660=CARTESIAN_POINT('Ctrl Pts',(-0.329362034481868,-0.159416832712907,
0.314473213303831));
#31661=CARTESIAN_POINT('Ctrl Pts',(-0.227729428899003,-0.286678573326201,
0.320945361203317));
#31662=CARTESIAN_POINT('Ctrl Pts',(-0.0809152203341978,-0.357609127112455,
0.327424927538347));
#31663=CARTESIAN_POINT('Ctrl Pts',(0.0823028008577847,-0.357312684079966,
0.333907107762849));
#31664=CARTESIAN_POINT('Ctrl Pts',(0.229369976399687,-0.286999416296364,
0.340400245782608));
#31665=CARTESIAN_POINT('Ctrl Pts',(0.331477217034357,-0.158117971828307,
0.346888605564388));
#31666=CARTESIAN_POINT('Ctrl Pts',(0.355417803964002,-0.0537733405890617,
0.351235961881927));
#31667=CARTESIAN_POINT('Ctrl Pts',(0.355614008397637,0.000526897379297947,
0.35339086956434));
#31668=CARTESIAN_POINT('Ctrl Pts',(0.323263761278146,0.0011652749059825,
0.00102359537366932));
#31669=CARTESIAN_POINT('Ctrl Pts',(0.32308388504024,0.0509466298067978,
0.00299917095282439));
#31670=CARTESIAN_POINT('Ctrl Pts',(0.301325186385381,0.145526233085643,
0.0069406494446651));
#31671=CARTESIAN_POINT('Ctrl Pts',(0.208169819552591,0.263398218702504,
0.0128703570176973));
#31672=CARTESIAN_POINT('Ctrl Pts',(0.0736352659440483,0.327653486273809,
0.0188072832941143));
#31673=CARTESIAN_POINT('Ctrl Pts',(-0.0760885903995774,0.328030617131512,
0.0247556929444235));
#31674=CARTESIAN_POINT('Ctrl Pts',(-0.211125322474165,0.262793911768754,
0.0307136354236982));
#31675=CARTESIAN_POINT('Ctrl Pts',(-0.30483335192296,0.145508174571446,
0.0366818386650944));
#31676=CARTESIAN_POINT('Ctrl Pts',(-0.332736604267165,0.0232418188678019,
0.0416639718287818));
#31677=CARTESIAN_POINT('Ctrl Pts',(-0.3230187894293,-0.0624385261228433,
0.0451558754794785));
#31678=CARTESIAN_POINT('Ctrl Pts',(-0.309430912508696,-0.10958390059491,
0.0471523807534524));
#31679=CARTESIAN_POINT('Ctrl Pts',(-0.275067160512545,-0.192765131089754,
0.0508142216208795));
#31680=CARTESIAN_POINT('Ctrl Pts',(-0.173384898218217,-0.30262257252764,
0.0566489427637022));
#31681=CARTESIAN_POINT('Ctrl Pts',(0.0273145804812777,-0.348359213768784,
0.0646675914287231));
#31682=CARTESIAN_POINT('Ctrl Pts',(0.203266956937511,-0.279400513558744,
0.0720353597363947));
#31683=CARTESIAN_POINT('Ctrl Pts',(0.308436007640621,-0.147165797018185,
0.0787463017504538));
#31684=CARTESIAN_POINT('Ctrl Pts',(0.342442191511722,0.00117726716011259,
0.0847965020332884));
#31685=CARTESIAN_POINT('Ctrl Pts',(0.308448294174871,0.149886349764988,
0.0908569625697496));
#31686=CARTESIAN_POINT('Ctrl Pts',(0.213279665334743,0.26936826303577,0.0969276519284122));
#31687=CARTESIAN_POINT('Ctrl Pts',(0.0754008583417468,0.335738815799705,
0.103008616752156));
#31688=CARTESIAN_POINT('Ctrl Pts',(-0.0779153548107563,0.335814356976075,
0.109099752247069));
#31689=CARTESIAN_POINT('Ctrl Pts',(-0.216159240659499,0.269204901675787,
0.115201143937647));
#31690=CARTESIAN_POINT('Ctrl Pts',(-0.312302840736801,0.148912374598733,
0.121312645115956));
#31691=CARTESIAN_POINT('Ctrl Pts',(-0.346163600796807,-0.00102923428505851,
0.127434365100191));
#31692=CARTESIAN_POINT('Ctrl Pts',(-0.301573902044757,-0.202360103152527,
0.135610016965582));
#31693=CARTESIAN_POINT('Ctrl Pts',(-0.0850566432589637,-0.375824958530099,
0.145855089726598));
#31694=CARTESIAN_POINT('Ctrl Pts',(0.241962386947492,-0.301799047216122,
0.158189044407346));
#31695=CARTESIAN_POINT('Ctrl Pts',(0.387828938012594,0.00131775672787745,
0.170562769165271));
#31696=CARTESIAN_POINT('Ctrl Pts',(0.266068485484251,0.253601605330286,
0.180906998748366));
#31697=CARTESIAN_POINT('Ctrl Pts',(0.0770061287527791,0.343252947438917,
0.189201773157529));
#31698=CARTESIAN_POINT('Ctrl Pts',(-0.0794446669689747,0.343662665319532,
0.195432501073281));
#31699=CARTESIAN_POINT('Ctrl Pts',(-0.221066126232674,0.275338906399848,
0.201672855000828));
#31700=CARTESIAN_POINT('Ctrl Pts',(-0.319144627584919,0.152499087945336,
0.207922683407449));
#31701=CARTESIAN_POINT('Ctrl Pts',(-0.354179786673318,-0.00110753927353714,
0.214182002780984));
#31702=CARTESIAN_POINT('Ctrl Pts',(-0.319166531156333,-0.154917399863823,
0.220450660338253));
#31703=CARTESIAN_POINT('Ctrl Pts',(-0.220637111918073,-0.278401206258936,
0.226728661851426));
#31704=CARTESIAN_POINT('Ctrl Pts',(-0.0781215508622231,-0.347159715044341,
0.233015834255785));
#31705=CARTESIAN_POINT('Ctrl Pts',(0.080287554663607,-0.347070588075095,
0.239312154857787));
#31706=CARTESIAN_POINT('Ctrl Pts',(0.239257652256424,-0.270773321076525,
0.246318192490788));
#31707=CARTESIAN_POINT('Ctrl Pts',(0.35093898589305,-0.107236396197418,
0.254037368004576));
#31708=CARTESIAN_POINT('Ctrl Pts',(0.351111227440523,0.10931883915664,0.262474266548859));
#31709=CARTESIAN_POINT('Ctrl Pts',(0.228833468081611,0.288535277900801,
0.270926380939377));
#31710=CARTESIAN_POINT('Ctrl Pts',(0.0266925824577831,0.368103565438035,
0.279393970650793));
#31711=CARTESIAN_POINT('Ctrl Pts',(-0.185696236216694,0.319645295407652,
0.287876328764416));
#31712=CARTESIAN_POINT('Ctrl Pts',(-0.321535144076036,0.173101071392216,
0.295665258245558));
#31713=CARTESIAN_POINT('Ctrl Pts',(-0.361082579337844,-0.000956223706756918,
0.302756882611919));
#31714=CARTESIAN_POINT('Ctrl Pts',(-0.32544517604417,-0.157762357732159,
0.309147439370426));
#31715=CARTESIAN_POINT('Ctrl Pts',(-0.224978122399143,-0.283567336452126,
0.315545488109766));
#31716=CARTESIAN_POINT('Ctrl Pts',(-0.0798082459991771,-0.353718739900048,
0.32195248587614));
#31717=CARTESIAN_POINT('Ctrl Pts',(0.0816387315204158,-0.353420513894944,
0.328364404520402));
#31718=CARTESIAN_POINT('Ctrl Pts',(0.227155226998822,-0.283871579779252,
0.334788486194004));
#31719=CARTESIAN_POINT('Ctrl Pts',(0.328215224283278,-0.156290050231924,
0.341210885809922));
#31720=CARTESIAN_POINT('Ctrl Pts',(0.351915021246625,-0.0530322184023736,
0.345513041507324));
#31721=CARTESIAN_POINT('Ctrl Pts',(0.35210941700762,0.000767463320028059,
0.347648084589869));
#31722=CARTESIAN_POINT('Ctrl Pts',(0.3143497770318,0.00100791399453752,
0.00417722082587345));
#31723=CARTESIAN_POINT('Ctrl Pts',(0.314174444955958,0.0495316567334979,
0.006102888002978));
#31724=CARTESIAN_POINT('Ctrl Pts',(0.293026748720441,0.141376025106581,
0.00993052643649342));
#31725=CARTESIAN_POINT('Ctrl Pts',(0.202454346374076,0.256059066455207,
0.0156981800761764));
#31726=CARTESIAN_POINT('Ctrl Pts',(0.0716524230376314,0.318486601600921,
0.0214690413557031));
#31727=CARTESIAN_POINT('Ctrl Pts',(-0.0739017686534995,0.31887794641969,
0.0272520660610699));
#31728=CARTESIAN_POINT('Ctrl Pts',(-0.205150715552183,0.255448411785207,
0.0330425408443067));
#31729=CARTESIAN_POINT('Ctrl Pts',(-0.296232579005206,0.141460288765413,
0.0388433659915622));
#31730=CARTESIAN_POINT('Ctrl Pts',(-0.323344939862462,0.0226317046800233,
0.0436848833441879));
#31731=CARTESIAN_POINT('Ctrl Pts',(-0.313899608979832,-0.060631936346867,
0.0470782603736746));
#31732=CARTESIAN_POINT('Ctrl Pts',(-0.300693617065818,-0.106451761520664,
0.0490185943697462));
#31733=CARTESIAN_POINT('Ctrl Pts',(-0.267296784696181,-0.187291053982876,
0.0525773313312681));
#31734=CARTESIAN_POINT('Ctrl Pts',(-0.168501916293235,-0.294031184492012,
0.0582458003866922));
#31735=CARTESIAN_POINT('Ctrl Pts',(0.0265217080425736,-0.338468900053865,
0.066037693415352));
#31736=CARTESIAN_POINT('Ctrl Pts',(0.197480954357712,-0.271470453852949,
0.0731959148965402));
#31737=CARTESIAN_POINT('Ctrl Pts',(0.299662458425762,-0.1429841872325,0.0797163664559953));
#31738=CARTESIAN_POINT('Ctrl Pts',(0.332707595799803,0.00114716748899207,
0.0855946560055489));
#31739=CARTESIAN_POINT('Ctrl Pts',(0.299673735812974,0.145633690283821,
0.0914829317886208));
#31740=CARTESIAN_POINT('Ctrl Pts',(0.207208825230489,0.261728500340961,
0.097381253187885));
#31741=CARTESIAN_POINT('Ctrl Pts',(0.0732372745429245,0.326212791260178,
0.103289636985298));
#31742=CARTESIAN_POINT('Ctrl Pts',(-0.0757368242826929,0.326290610457155,
0.109208166354362));
#31743=CARTESIAN_POINT('Ctrl Pts',(-0.210069264644612,0.261561190313174,
0.115136835302027));
#31744=CARTESIAN_POINT('Ctrl Pts',(-0.303501461520976,0.144667206221031,
0.121075735274062));
#31745=CARTESIAN_POINT('Ctrl Pts',(-0.33640552849753,-0.00105114360770151,
0.127024838842762));
#31746=CARTESIAN_POINT('Ctrl Pts',(-0.293071888244684,-0.196725338364434,
0.134970722603791));
#31747=CARTESIAN_POINT('Ctrl Pts',(-0.0826205547868334,-0.365337759369106,
0.144928659779304));
#31748=CARTESIAN_POINT('Ctrl Pts',(0.235308544687022,-0.293385579417626,
0.156919602308117));
#31749=CARTESIAN_POINT('Ctrl Pts',(0.377167918354085,0.00136502922110808,
0.168951937351355));
#31750=CARTESIAN_POINT('Ctrl Pts',(0.258748526764981,0.246762198818122,
0.179013431660086));
#31751=CARTESIAN_POINT('Ctrl Pts',(0.0748100498926877,0.333987556781711,
0.187083384029882));
#31752=CARTESIAN_POINT('Ctrl Pts',(-0.0774247661752075,0.334388365324906,
0.193146211385528));
#31753=CARTESIAN_POINT('Ctrl Pts',(-0.215253722800486,0.267896699637554,
0.199219373691256));
#31754=CARTESIAN_POINT('Ctrl Pts',(-0.310723951021264,0.148327693877378,
0.205302893635305));
#31755=CARTESIAN_POINT('Ctrl Pts',(-0.344835425098166,-0.0012174970511246,
0.211396712812984));
#31756=CARTESIAN_POINT('Ctrl Pts',(-0.310743621977528,-0.150990654519629,
0.217500860527999));
#31757=CARTESIAN_POINT('Ctrl Pts',(-0.214783997648992,-0.271259017547068,
0.22361526923801));
#31758=CARTESIAN_POINT('Ctrl Pts',(-0.0759539911741114,-0.338242375219202,
0.229739944634851));
#31759=CARTESIAN_POINT('Ctrl Pts',(0.0783932441541543,-0.338159167803166,
0.235874832502872));
#31760=CARTESIAN_POINT('Ctrl Pts',(0.233321229982812,-0.263805853805254,
0.24270269913196));
#31761=CARTESIAN_POINT('Ctrl Pts',(0.342201575184436,-0.104386212514232,
0.250227870691107));
#31762=CARTESIAN_POINT('Ctrl Pts',(0.342377862772396,0.10678419186207,0.258455044914927));
#31763=CARTESIAN_POINT('Ctrl Pts',(0.223106451745026,0.281615630068196,
0.266700149646066));
#31764=CARTESIAN_POINT('Ctrl Pts',(0.0258611457879684,0.359265028954348,
0.274962893164122));
#31765=CARTESIAN_POINT('Ctrl Pts',(-0.181471173906832,0.311975315176289,
0.283243312867527));
#31766=CARTESIAN_POINT('Ctrl Pts',(-0.314129400185778,0.168869863676765,
0.290849825356883));
#31767=CARTESIAN_POINT('Ctrl Pts',(-0.352767893347067,-0.0011524177295687,
0.297777211902988));
#31768=CARTESIAN_POINT('Ctrl Pts',(-0.317947143101735,-0.154378046283838,
0.304021816820379));
#31769=CARTESIAN_POINT('Ctrl Pts',(-0.219751851958905,-0.2773449048768,
0.310275672881377));
#31770=CARTESIAN_POINT('Ctrl Pts',(-0.0778177620146979,-0.345946144519262,
0.316539857977124));
#31771=CARTESIAN_POINT('Ctrl Pts',(0.0800916001784434,-0.345646777099896,
0.322811784793249));
#31772=CARTESIAN_POINT('Ctrl Pts',(0.222457203835381,-0.277635516145105,
0.329095893848701));
#31773=CARTESIAN_POINT('Ctrl Pts',(0.321375732078151,-0.152720989873198,
0.335383674313783));
#31774=CARTESIAN_POINT('Ctrl Pts',(0.344583361544119,-0.0517156352897094,
0.339592387805982));
#31775=CARTESIAN_POINT('Ctrl Pts',(0.344773950821541,0.00103058928075043,
0.341685624388322));
#31776=CARTESIAN_POINT('Ctrl Pts',(0.301487309249758,0.000456552091686937,
0.0168995335103255));
#31777=CARTESIAN_POINT('Ctrl Pts',(0.301318644157645,0.0471351846205436,
0.0187519773957139));
#31778=CARTESIAN_POINT('Ctrl Pts',(0.2810381206102,0.135021677602031,0.0224153073649692));
#31779=CARTESIAN_POINT('Ctrl Pts',(0.194239037473508,0.245007882920672,
0.027945676794797));
#31780=CARTESIAN_POINT('Ctrl Pts',(0.0689981063776347,0.304715578239823,
0.0334693902717626));
#31781=CARTESIAN_POINT('Ctrl Pts',(-0.0702900555082151,0.305109671029292,
0.0390042903358426));
#31782=CARTESIAN_POINT('Ctrl Pts',(-0.195787398577806,0.244427515329891,
0.044540988571053));
#31783=CARTESIAN_POINT('Ctrl Pts',(-0.282824724120957,0.135496598851049,
0.0500848449251036));
#31784=CARTESIAN_POINT('Ctrl Pts',(-0.308711795376669,0.0219958303263355,
0.0547090024061654));
#31785=CARTESIAN_POINT('Ctrl Pts',(-0.29969420448995,-0.0574925396160197,
0.0579486413010252));
#31786=CARTESIAN_POINT('Ctrl Pts',(-0.287089894521034,-0.101224391094012,
0.0598005555602701));
#31787=CARTESIAN_POINT('Ctrl Pts',(-0.255219231588607,-0.178368997813358,
0.0631966456490891));
#31788=CARTESIAN_POINT('Ctrl Pts',(-0.160958434699617,-0.280185707839856,
0.0686045510379543));
#31789=CARTESIAN_POINT('Ctrl Pts',(0.0249425970611792,-0.322526026192247,
0.0760318037970623));
#31790=CARTESIAN_POINT('Ctrl Pts',(0.187788206134099,-0.258686428390149,
0.0828508087168802));
#31791=CARTESIAN_POINT('Ctrl Pts',(0.285061784518795,-0.136361708668944,
0.0890584674717641));
#31792=CARTESIAN_POINT('Ctrl Pts',(0.316497406441131,0.000792437315105745,
0.0946521949347518));
#31793=CARTESIAN_POINT('Ctrl Pts',(0.28507324950853,0.138219078024721,0.100252882809767));
#31794=CARTESIAN_POINT('Ctrl Pts',(0.197156599915038,0.248588740509545,
0.105860686505017));
#31795=CARTESIAN_POINT('Ctrl Pts',(0.0698367774737854,0.309867367627101,
0.111475746073964));
#31796=CARTESIAN_POINT('Ctrl Pts',(-0.0716830353582476,0.309933053031314,
0.117098178038573));
#31797=CARTESIAN_POINT('Ctrl Pts',(-0.199244451681163,0.248462891041503,
0.122728160853189));
#31798=CARTESIAN_POINT('Ctrl Pts',(-0.287930342488211,0.137494903576697,
0.128365781293317));
#31799=CARTESIAN_POINT('Ctrl Pts',(-0.319152161969064,-0.000783574171537168,
0.134011240827325));
#31800=CARTESIAN_POINT('Ctrl Pts',(-0.278035089510408,-0.18640701314818,
0.141548997600109));
#31801=CARTESIAN_POINT('Ctrl Pts',(-0.0784631926776667,-0.346266505185913,
0.150991489427036));
#31802=CARTESIAN_POINT('Ctrl Pts',(0.222836755126196,-0.278041772009318,
0.162355555259985));
#31803=CARTESIAN_POINT('Ctrl Pts',(0.357193668716545,0.00118449665979845,
0.17375385635394));
#31804=CARTESIAN_POINT('Ctrl Pts',(0.2450404452584,0.23355531905656,0.183281617763114));
#31805=CARTESIAN_POINT('Ctrl Pts',(0.0708989045308578,0.316131965777688,
0.190921795813857));
#31806=CARTESIAN_POINT('Ctrl Pts',(-0.0732099472936145,0.316509785082592,
0.196660991057498));
#31807=CARTESIAN_POINT('Ctrl Pts',(-0.203667301369978,0.253573050762465,
0.202409381813254));
#31808=CARTESIAN_POINT('Ctrl Pts',(-0.294022688408376,0.140408123958125,
0.208167033486851));
#31809=CARTESIAN_POINT('Ctrl Pts',(-0.326304383791802,-0.0011172174790417,
0.213934077022798));
#31810=CARTESIAN_POINT('Ctrl Pts',(-0.294042134324106,-0.142850802528825,
0.219710546097136));
#31811=CARTESIAN_POINT('Ctrl Pts',(-0.203236242617689,-0.256659822856353,
0.225496572304767));
#31812=CARTESIAN_POINT('Ctrl Pts',(-0.0718641880841615,-0.320045263581161,
0.231292227048866));
#31813=CARTESIAN_POINT('Ctrl Pts',(0.0741925396792679,-0.319966890116769,
0.237097594375026));
#31814=CARTESIAN_POINT('Ctrl Pts',(0.22080328921599,-0.249606394849742,
0.243558861586279));
#31815=CARTESIAN_POINT('Ctrl Pts',(0.323844093963753,-0.0987405175598124,
0.250680303919329));
#31816=CARTESIAN_POINT('Ctrl Pts',(0.32401507287333,0.101121051148882,0.258466870226901));
#31817=CARTESIAN_POINT('Ctrl Pts',(0.211121630360006,0.266610552139869,
0.266271226345274));
#31818=CARTESIAN_POINT('Ctrl Pts',(0.0243894520669469,0.340127943927118,
0.274093646786023));
#31819=CARTESIAN_POINT('Ctrl Pts',(-0.17192978881275,0.295356272268269,
0.28193413025846));
#31820=CARTESIAN_POINT('Ctrl Pts',(-0.297574955055663,0.159828459938204,
0.289137905336518));
#31821=CARTESIAN_POINT('Ctrl Pts',(-0.334179435288708,-0.0012318952504744,
0.295700328362607));
#31822=CARTESIAN_POINT('Ctrl Pts',(-0.301195173483201,-0.146417950178875,
0.301616739917366));
#31823=CARTESIAN_POINT('Ctrl Pts',(-0.208135055759231,-0.262944613995742,
0.307543700779419));
#31824=CARTESIAN_POINT('Ctrl Pts',(-0.0736043148012352,-0.328002669716722,
0.313480824491926));
#31825=CARTESIAN_POINT('Ctrl Pts',(0.0761330634504403,-0.327682926701522,
0.319429011228321));
#31826=CARTESIAN_POINT('Ctrl Pts',(0.211157784923481,-0.263255004979861,
0.325386838675828));
#31827=CARTESIAN_POINT('Ctrl Pts',(0.305008353090155,-0.144615638098925,
0.331356623228847));
#31828=CARTESIAN_POINT('Ctrl Pts',(0.327024456208159,-0.0489885211905165,
0.335341847701417));
#31829=CARTESIAN_POINT('Ctrl Pts',(0.327206044585182,0.00126667387289164,
0.337336227652134));
#31830=CARTESIAN_POINT('Ctrl Pts',(0.296534826482144,-0.000422773883966688,
0.0386062224122653));
#31831=CARTESIAN_POINT('Ctrl Pts',(0.296368800707151,0.0455254187392618,
0.0404296787531709));
#31832=CARTESIAN_POINT('Ctrl Pts',(0.276427070000758,0.131843682442671,
0.0440279011289847));
#31833=CARTESIAN_POINT('Ctrl Pts',(0.191202125564478,0.23985144495526,0.0494584217321202));
#31834=CARTESIAN_POINT('Ctrl Pts',(0.0684086392330356,0.298341986007322,
0.0548730358166816));
#31835=CARTESIAN_POINT('Ctrl Pts',(-0.0679772583367851,0.298725491344516,
0.0602928330160072));
#31836=CARTESIAN_POINT('Ctrl Pts',(-0.19068103897547,0.239358210205861,
0.0657064966754378));
#31837=CARTESIAN_POINT('Ctrl Pts',(-0.275669308368296,0.132968726389537,
0.0711207302467392));
#31838=CARTESIAN_POINT('Ctrl Pts',(-0.300900441972001,0.0222585036177047,
0.0756307716387691));
#31839=CARTESIAN_POINT('Ctrl Pts',(-0.292110160241601,-0.0551960737139081,
0.0787875627319099));
#31840=CARTESIAN_POINT('Ctrl Pts',(-0.279833018161878,-0.0977913812013095,
0.0805913361942464));
#31841=CARTESIAN_POINT('Ctrl Pts',(-0.248799516171456,-0.172907063390399,
0.0838980938896731));
#31842=CARTESIAN_POINT('Ctrl Pts',(-0.157090879780932,-0.271919338836937,
0.0891579601221785));
#31843=CARTESIAN_POINT('Ctrl Pts',(0.023450493308891,-0.312990434018135,
0.0963707260335879));
#31844=CARTESIAN_POINT('Ctrl Pts',(0.18131798103562,-0.25106041949659,0.102981727384833));
#31845=CARTESIAN_POINT('Ctrl Pts',(0.275476413276219,-0.132616711396579,
0.108991757135753));
#31846=CARTESIAN_POINT('Ctrl Pts',(0.305859403306453,1.75294825909618E-5,
0.114400912598483));
#31847=CARTESIAN_POINT('Ctrl Pts',(0.275488262452244,0.132749583053741,
0.11981042719508));
#31848=CARTESIAN_POINT('Ctrl Pts',(0.190657413586372,0.239219379063661,
0.125220540905927));
#31849=CARTESIAN_POINT('Ctrl Pts',(0.0679580198860075,0.298252809245818,
0.130631420428721));
#31850=CARTESIAN_POINT('Ctrl Pts',(-0.0682628639615764,0.298299872442762,
0.136043298037454));
#31851=CARTESIAN_POINT('Ctrl Pts',(-0.190903109853683,0.239181080607407,
0.141456373034151));
#31852=CARTESIAN_POINT('Ctrl Pts',(-0.276065680943723,0.132593720175959,
0.146870863206197));
#31853=CARTESIAN_POINT('Ctrl Pts',(-0.306004572638831,-7.02355279394243E-5,
0.15228698901937));
#31854=CARTESIAN_POINT('Ctrl Pts',(-0.266572495720376,-0.177966792725148,
0.159510876102804));
#31855=CARTESIAN_POINT('Ctrl Pts',(-0.0755420141437979,-0.330844040968773,
0.168545866717772));
#31856=CARTESIAN_POINT('Ctrl Pts',(0.212146858309987,-0.265560948222135,
0.179397548526666));
#31857=CARTESIAN_POINT('Ctrl Pts',(0.340075411028669,0.000609232641378717,
0.19026070926692));
#31858=CARTESIAN_POINT('Ctrl Pts',(0.233301287065815,0.221612007646323,
0.199324114439432));
#31859=CARTESIAN_POINT('Ctrl Pts',(0.0678658260526744,0.300036005250322,
0.206582184805351));
#31860=CARTESIAN_POINT('Ctrl Pts',(-0.0689173179449983,0.300383347622569,
0.212029566572711));
#31861=CARTESIAN_POINT('Ctrl Pts',(-0.1926289646447,0.240684814109104,0.217480994418533));
#31862=CARTESIAN_POINT('Ctrl Pts',(-0.278235295212214,0.133447490935984,
0.222936674155516));
#31863=CARTESIAN_POINT('Ctrl Pts',(-0.30878671001653,-0.000548565157992426,
0.228396798149705));
#31864=CARTESIAN_POINT('Ctrl Pts',(-0.278253232166184,-0.13463029520536,
0.233861524378761));
#31865=CARTESIAN_POINT('Ctrl Pts',(-0.192405461785685,-0.242206618549997,
0.239331056898387));
#31866=CARTESIAN_POINT('Ctrl Pts',(-0.0683064866778343,-0.302069560502724,
0.244805628557127));
#31867=CARTESIAN_POINT('Ctrl Pts',(0.0695574987923262,-0.301984756295867,
0.250285393496364));
#31868=CARTESIAN_POINT('Ctrl Pts',(0.207841992242269,-0.235606303949781,
0.25637992006153));
#31869=CARTESIAN_POINT('Ctrl Pts',(0.304940375421062,-0.0934010154145467,
0.26309199604083));
#31870=CARTESIAN_POINT('Ctrl Pts',(0.305076348451544,0.0948036199515923,
0.270424418777817));
#31871=CARTESIAN_POINT('Ctrl Pts',(0.198835199181958,0.25050195808659,0.277767683891008));
#31872=CARTESIAN_POINT('Ctrl Pts',(0.0232685326754069,0.319598579521238,
0.285122049639541));
#31873=CARTESIAN_POINT('Ctrl Pts',(-0.161163670412757,0.277517849683546,
0.292488048692369));
#31874=CARTESIAN_POINT('Ctrl Pts',(-0.279108455532343,0.150266199480721,
0.299251126448657));
#31875=CARTESIAN_POINT('Ctrl Pts',(-0.313444344793882,-0.00084859398882846,
0.305408493993884));
#31876=CARTESIAN_POINT('Ctrl Pts',(-0.282505268282257,-0.137014310816318,
0.310956928179577));
#31877=CARTESIAN_POINT('Ctrl Pts',(-0.195261921712917,-0.246230960103103,
0.316513236752478));
#31878=CARTESIAN_POINT('Ctrl Pts',(-0.0692111802430976,-0.307213573846843,
0.322075524046817));
#31879=CARTESIAN_POINT('Ctrl Pts',(0.0710557555603892,-0.306861663537198,
0.327648701198013));
#31880=CARTESIAN_POINT('Ctrl Pts',(0.197474063293807,-0.246618398330353,
0.333224270871386));
#31881=CARTESIAN_POINT('Ctrl Pts',(0.285319369726677,-0.135402277387047,
0.338817890656192));
#31882=CARTESIAN_POINT('Ctrl Pts',(0.305907629221196,-0.0462097653749184,
0.342535764331766));
#31883=CARTESIAN_POINT('Ctrl Pts',(0.306078438298251,0.00106222211004659,
0.344411755539274));
#31884=CARTESIAN_POINT('Ctrl Pts',(0.315101647298455,-0.00128170895505734,
0.0619405265894516));
#31885=CARTESIAN_POINT('Ctrl Pts',(0.31492625461718,0.0472588065417078,
0.0638668593942953));
#31886=CARTESIAN_POINT('Ctrl Pts',(0.293727533658683,0.139191100388604,
0.0676985669032832));
#31887=CARTESIAN_POINT('Ctrl Pts',(0.203343654855236,0.253543873366989,
0.073451247670091));
#31888=CARTESIAN_POINT('Ctrl Pts',(0.0733096721848766,0.315539064523512,
0.0791872665185006));
#31889=CARTESIAN_POINT('Ctrl Pts',(-0.0708947358221901,0.315877322819963,
0.0849167160876448));
#31890=CARTESIAN_POINT('Ctrl Pts',(-0.200459890912327,0.253197165795973,
0.0906340723155647));
#31891=CARTESIAN_POINT('Ctrl Pts',(-0.290049959442992,0.140992188597427,
0.0963425721181722));
#31892=CARTESIAN_POINT('Ctrl Pts',(-0.316598605249467,0.0244332032193379,
0.101091233310832));
#31893=CARTESIAN_POINT('Ctrl Pts',(-0.307350474919786,-0.0570254397486972,
0.104411192517556));
#31894=CARTESIAN_POINT('Ctrl Pts',(-0.294446049587025,-0.101795700206291,
0.10630710240828));
#31895=CARTESIAN_POINT('Ctrl Pts',(-0.261838458042338,-0.180719311846423,
0.109781473180646));
#31896=CARTESIAN_POINT('Ctrl Pts',(-0.165560810784372,-0.284601056523487,
0.115301664113939));
#31897=CARTESIAN_POINT('Ctrl Pts',(0.0235312279036465,-0.327555783312208,
0.122855538346143));
#31898=CARTESIAN_POINT('Ctrl Pts',(0.188503486018219,-0.262779385929021,
0.129764974303623));
#31899=CARTESIAN_POINT('Ctrl Pts',(0.286705132748725,-0.139203688799005,
0.136034616453424));
#31900=CARTESIAN_POINT('Ctrl Pts',(0.318325171185559,-0.00105509771065233,
0.141668412008706));
#31901=CARTESIAN_POINT('Ctrl Pts',(0.286719151798664,0.136958826184427,
0.14729347124296));
#31902=CARTESIAN_POINT('Ctrl Pts',(0.198632022686421,0.247473183495014,
0.152909932970554));
#31903=CARTESIAN_POINT('Ctrl Pts',(0.0714522871931054,0.308633723483916,
0.158517935270725));
#31904=CARTESIAN_POINT('Ctrl Pts',(-0.0694953492578695,0.308655272195571,
0.164117604325348));
#31905=CARTESIAN_POINT('Ctrl Pts',(-0.196166722112865,0.247565229485892,
0.169709114510168));
#31906=CARTESIAN_POINT('Ctrl Pts',(-0.283964270870719,0.137632576727079,
0.175292584482011));
#31907=CARTESIAN_POINT('Ctrl Pts',(-0.31476265528893,0.00106015217748537,
0.180868211582949));
#31908=CARTESIAN_POINT('Ctrl Pts',(-0.274193925446901,-0.181763087900732,
0.188292028653664));
#31909=CARTESIAN_POINT('Ctrl Pts',(-0.0782674021616253,-0.338319258809273,
0.197552960595143));
#31910=CARTESIAN_POINT('Ctrl Pts',(0.21553531409664,-0.271395910669738,
0.208637010915907));
#31911=CARTESIAN_POINT('Ctrl Pts',(0.345513151112905,-0.00038789181246443,
0.219693495439871));
#31912=CARTESIAN_POINT('Ctrl Pts',(0.237056710850022,0.223658672152894,
0.228885208413172));
#31913=CARTESIAN_POINT('Ctrl Pts',(0.0697234149934862,0.302932208439939,
0.236226210010088));
#31914=CARTESIAN_POINT('Ctrl Pts',(-0.0683760040706116,0.303260211496953,
0.241725864636005));
#31915=CARTESIAN_POINT('Ctrl Pts',(-0.19303555845014,0.243069649037974,
0.247219669375935));
#31916=CARTESIAN_POINT('Ctrl Pts',(-0.27913043167095,0.135177892286265,
0.252707771531946));
#31917=CARTESIAN_POINT('Ctrl Pts',(-0.309779544180159,0.000622981248504958,
0.258190394873152));
#31918=CARTESIAN_POINT('Ctrl Pts',(-0.279149094048921,-0.133761341722244,
0.263667655624343));
#31919=CARTESIAN_POINT('Ctrl Pts',(-0.193238240682731,-0.241370806381079,
0.269139780151241));
#31920=CARTESIAN_POINT('Ctrl Pts',(-0.0692929091135377,-0.301128915488362,
0.274606991419976));
#31921=CARTESIAN_POINT('Ctrl Pts',(0.0681349598665013,-0.301016236101523,
0.2800694292738));
#31922=CARTESIAN_POINT('Ctrl Pts',(0.205722480619705,-0.234937901808181,
0.286133732978082));
#31923=CARTESIAN_POINT('Ctrl Pts',(0.302082544121992,-0.093704256729346,
0.292798181344527));
#31924=CARTESIAN_POINT('Ctrl Pts',(0.302150472949551,0.0927223497626265,
0.300061261848913));
#31925=CARTESIAN_POINT('Ctrl Pts',(0.19711290358951,0.246534520123679,0.307317361175983));
#31926=CARTESIAN_POINT('Ctrl Pts',(0.024014651371324,0.314590469125311,
0.314567245913451));
#31927=CARTESIAN_POINT('Ctrl Pts',(-0.157345516009493,0.273139119421548,
0.321811112240196));
#31928=CARTESIAN_POINT('Ctrl Pts',(-0.273017499230799,0.148255125916073,
0.328446171918567));
#31929=CARTESIAN_POINT('Ctrl Pts',(-0.306603925817584,0.000295637397937573,
0.334474828088449));
#31930=CARTESIAN_POINT('Ctrl Pts',(-0.276342099141224,-0.132785077310565,
0.339897459977899));
#31931=CARTESIAN_POINT('Ctrl Pts',(-0.191200427627164,-0.239318641719874,
0.345318556602232));
#31932=CARTESIAN_POINT('Ctrl Pts',(-0.0684258001418649,-0.298703158508728,
0.350735481649343));
#31933=CARTESIAN_POINT('Ctrl Pts',(0.0679566655576182,-0.298312240153081,
0.356154839923386));
#31934=CARTESIAN_POINT('Ctrl Pts',(0.190650317768282,-0.239856073740776,
0.361565262555767));
#31935=CARTESIAN_POINT('Ctrl Pts',(0.275745802382817,-0.131995078166987,
0.366987994062727));
#31936=CARTESIAN_POINT('Ctrl Pts',(0.295638197983241,-0.045872517774112,
0.370578103976212));
#31937=CARTESIAN_POINT('Ctrl Pts',(0.295803909517168,-1.12925223861182E-5,
0.372398109013342));
#31938=CARTESIAN_POINT('Ctrl Pts',(0.344894607025859,-0.00117220091143172,
0.0618937486917298));
#31939=CARTESIAN_POINT('Ctrl Pts',(0.344703966040985,0.051588333982661,
0.0639875531791247));
#31940=CARTESIAN_POINT('Ctrl Pts',(0.321489911562902,0.152620094193498,
0.0681973923342701));
#31941=CARTESIAN_POINT('Ctrl Pts',(0.22256664720873,0.277542883006417,0.0744854517154489));
#31942=CARTESIAN_POINT('Ctrl Pts',(0.0802116976126469,0.345540567216692,
0.0807688522723124));
#31943=CARTESIAN_POINT('Ctrl Pts',(-0.0776391716305396,0.345840974720998,
0.087038807205936));
#31944=CARTESIAN_POINT('Ctrl Pts',(-0.219508915025033,0.277260432316066,
0.0932998185216175));
#31945=CARTESIAN_POINT('Ctrl Pts',(-0.317591755286808,0.154390861205383,
0.0995493368234934));
#31946=CARTESIAN_POINT('Ctrl Pts',(-0.346661039759245,0.0267922753448241,
0.104748509576963));
#31947=CARTESIAN_POINT('Ctrl Pts',(-0.336535485770271,-0.0623898119372897,
0.108383100293887));
#31948=CARTESIAN_POINT('Ctrl Pts',(-0.322408424731889,-0.111401720018576,
0.110458667643685));
#31949=CARTESIAN_POINT('Ctrl Pts',(-0.286711444159767,-0.197802933078996,
0.114262205448296));
#31950=CARTESIAN_POINT('Ctrl Pts',(-0.181320545975211,-0.311512954024223,
0.120304748022494));
#31951=CARTESIAN_POINT('Ctrl Pts',(0.0256366134017508,-0.358518960303294,
0.128572221561375));
#31952=CARTESIAN_POINT('Ctrl Pts',(0.206149878169194,-0.287632860671769,
0.136132629991281));
#31953=CARTESIAN_POINT('Ctrl Pts',(0.313573318790257,-0.152444007237616,
0.142991291085792));
#31954=CARTESIAN_POINT('Ctrl Pts',(0.348151986684333,-0.00135155530985844,
0.149152888630487));
#31955=CARTESIAN_POINT('Ctrl Pts',(0.313588656288107,0.14954981179416,0.155303241992947));
#31956=CARTESIAN_POINT('Ctrl Pts',(0.217300641502055,0.270344572766772,
0.161442322103795));
#31957=CARTESIAN_POINT('Ctrl Pts',(0.0783302437237461,0.33716785546378,
0.167570083359719));
#31958=CARTESIAN_POINT('Ctrl Pts',(-0.0756245191684134,0.337184670947358,
0.173686512217792));
#31959=CARTESIAN_POINT('Ctrl Pts',(-0.213926786047297,0.270477291973825,
0.179791561237685));
#31960=CARTESIAN_POINT('Ctrl Pts',(-0.309740427769701,0.150493872976662,
0.185885228264861));
#31961=CARTESIAN_POINT('Ctrl Pts',(-0.3433301135152,0.00151097286038558,
0.191967471988919));
#31962=CARTESIAN_POINT('Ctrl Pts',(-0.299082473709324,-0.197828041114981,
0.200061909718623));
#31963=CARTESIAN_POINT('Ctrl Pts',(-0.0855849665151933,-0.368340181506443,
0.210151340739428));
#31964=CARTESIAN_POINT('Ctrl Pts',(0.234108819111557,-0.295422317233866,
0.222212862825778));
#31965=CARTESIAN_POINT('Ctrl Pts',(0.375268601750312,-0.000857533008588078,
0.234228580964883));
#31966=CARTESIAN_POINT('Ctrl Pts',(0.25749264156393,0.242240410083148,0.24420359765261));
#31967=CARTESIAN_POINT('Ctrl Pts',(0.076109197473031,0.328146093635365,
0.252160795683558));
#31968=CARTESIAN_POINT('Ctrl Pts',(-0.0734630576993165,0.328488983850561,
0.258117334003062));
#31969=CARTESIAN_POINT('Ctrl Pts',(-0.208357730141545,0.263339735952782,
0.264062515706671));
#31970=CARTESIAN_POINT('Ctrl Pts',(-0.301433211455292,0.146675275774542,
0.269996393190013));
#31971=CARTESIAN_POINT('Ctrl Pts',(-0.334527391943304,0.00131958428967035,
0.275918982746397));
#31972=CARTESIAN_POINT('Ctrl Pts',(-0.30145311065115,-0.143710382389741,
0.281830329757323));
#31973=CARTESIAN_POINT('Ctrl Pts',(-0.208811314453104,-0.25972617686706,
0.287730466702406));
#31974=CARTESIAN_POINT('Ctrl Pts',(-0.0752963160901684,-0.324078250133092,
0.293619451824586));
#31975=CARTESIAN_POINT('Ctrl Pts',(0.0725822231329485,-0.323940922408941,
0.299497337556348));
#31976=CARTESIAN_POINT('Ctrl Pts',(0.220469193575753,-0.252893157585676,
0.306015977608672));
#31977=CARTESIAN_POINT('Ctrl Pts',(0.323888963496138,-0.101243997194457,
0.313170937392681));
#31978=CARTESIAN_POINT('Ctrl Pts',(0.323914718356231,0.0986015513486016,
0.320956782079779));
#31979=CARTESIAN_POINT('Ctrl Pts',(0.211450301619867,0.263207970933167,
0.328723492520748));
#31980=CARTESIAN_POINT('Ctrl Pts',(0.0264517346568824,0.335890378755159,
0.336471005872168));
#31981=CARTESIAN_POINT('Ctrl Pts',(-0.167033447139801,0.291616636207715,
0.344199700797049));
#31982=CARTESIAN_POINT('Ctrl Pts',(-0.290203018169231,0.158568415055973,
0.35126714050295));
#31983=CARTESIAN_POINT('Ctrl Pts',(-0.325900520055194,0.00120617226061592,
0.35767858494089));
#31984=CARTESIAN_POINT('Ctrl Pts',(-0.29373299888089,-0.140130990161181,
0.363438374653413));
#31985=CARTESIAN_POINT('Ctrl Pts',(-0.203410557114407,-0.253129387443769,
0.369188308457246));
#31986=CARTESIAN_POINT('Ctrl Pts',(-0.0733398244589557,-0.315984228529682,
0.374927114369164));
#31987=CARTESIAN_POINT('Ctrl Pts',(0.070907119541957,-0.315592776376067,
0.380658098012618));
#31988=CARTESIAN_POINT('Ctrl Pts',(0.200499120082281,-0.253747220752294,
0.386375419790931));
#31989=CARTESIAN_POINT('Ctrl Pts',(0.290231966152725,-0.14011003674842,
0.392090289367516));
#31990=CARTESIAN_POINT('Ctrl Pts',(0.311180051930582,-0.0491735403917148,
0.395880310107509));
#31991=CARTESIAN_POINT('Ctrl Pts',(0.311353847170781,-0.00107512219721069,
0.397789098259406));
#31992=CARTESIAN_POINT('Ctrl Pts',(0.36349947386268,-0.000182513280454622,
0.0386491721592961));
#31993=CARTESIAN_POINT('Ctrl Pts',(0.363299197931637,0.0552445254292098,
0.0408487969850539));
#31994=CARTESIAN_POINT('Ctrl Pts',(0.338822849801048,0.162017987113332,
0.0452971626933041));
#31995=CARTESIAN_POINT('Ctrl Pts',(0.234401841864732,0.293778560944321,
0.0519311472688644));
#31996=CARTESIAN_POINT('Ctrl Pts',(0.0839251224276196,0.365759381145584,
0.0585757604749919));
#31997=CARTESIAN_POINT('Ctrl Pts',(-0.0831258602463933,0.366054544758465,
0.0652102611487041));
#31998=CARTESIAN_POINT('Ctrl Pts',(-0.233480113083901,0.293431779736776,
0.0718457140698859));
#31999=CARTESIAN_POINT('Ctrl Pts',(-0.337548697207091,0.163079909212871,
0.0784755564546323));
#32000=CARTESIAN_POINT('Ctrl Pts',(-0.368445531345481,0.0275650217023474,
0.0839980235483959));
#32001=CARTESIAN_POINT('Ctrl Pts',(-0.357684839286351,-0.0672426651280164,
0.0878617768994511));
#32002=CARTESIAN_POINT('Ctrl Pts',(-0.342661576869175,-0.119365372087535,
0.0900691038896605));
#32003=CARTESIAN_POINT('Ctrl Pts',(-0.304688860407797,-0.211277600934222,
0.0941152586155943));
#32004=CARTESIAN_POINT('Ctrl Pts',(-0.192498270408811,-0.332377332372952,
0.100549392864518));
#32005=CARTESIAN_POINT('Ctrl Pts',(0.0281733882059037,-0.382550621286202,
0.109365111791553));
#32006=CARTESIAN_POINT('Ctrl Pts',(0.220954062612933,-0.306893333992967,
0.11743876178892));
#32007=CARTESIAN_POINT('Ctrl Pts',(0.335829202294293,-0.162364653417003,
0.12477195777997));
#32008=CARTESIAN_POINT('Ctrl Pts',(0.372856255837749,-0.000655007332560676,
0.131366750230641));
#32009=CARTESIAN_POINT('Ctrl Pts',(0.335844870938437,0.161025293563643,
0.137956255408633));
#32010=CARTESIAN_POINT('Ctrl Pts',(0.232592962625393,0.290584863175236,
0.144540250872817));
#32011=CARTESIAN_POINT('Ctrl Pts',(0.0834124279892051,0.362339037782258,
0.151118603972318));
#32012=CARTESIAN_POINT('Ctrl Pts',(-0.0820214421351618,0.362374494803792,
0.157691097018862));
#32013=CARTESIAN_POINT('Ctrl Pts',(-0.230783736935749,0.290641660029172,
0.164257575225425));
#32014=CARTESIAN_POINT('Ctrl Pts',(-0.333948068275454,0.161482550546205,
0.170817836066568));
#32015=CARTESIAN_POINT('Ctrl Pts',(-0.370156587532269,0.00094904835990728,
0.17737170980749));
#32016=CARTESIAN_POINT('Ctrl Pts',(-0.322463302031498,-0.214034687891742,
0.186101501609228));
#32017=CARTESIAN_POINT('Ctrl Pts',(-0.0919790405353035,-0.398250109605909,
0.196996893196212));
#32018=CARTESIAN_POINT('Ctrl Pts',(0.253842468120618,-0.31950787991112,
0.210043175686943));
#32019=CARTESIAN_POINT('Ctrl Pts',(0.406874486079669,-0.000451865866853843,
0.223059865384761));
#32020=CARTESIAN_POINT('Ctrl Pts',(0.27918181167757,0.263318543608872,0.233881466919701));
#32021=CARTESIAN_POINT('Ctrl Pts',(0.0822068433707472,0.356629457468139,
0.242522733897225));
#32022=CARTESIAN_POINT('Ctrl Pts',(-0.0803281279023186,0.357012622815529,
0.248995529534002));
#32023=CARTESIAN_POINT('Ctrl Pts',(-0.227011595006363,0.286182978182527,
0.255460035897147));
#32024=CARTESIAN_POINT('Ctrl Pts',(-0.3282873008575,0.159258591210816,0.261916079613041));
#32025=CARTESIAN_POINT('Ctrl Pts',(-0.364323816221617,0.00102235932660949,
0.268363542385575));
#32026=CARTESIAN_POINT('Ctrl Pts',(-0.3283094791852,-0.156949994186001,
0.274802294072678));
#32027=CARTESIAN_POINT('Ctrl Pts',(-0.227355336560919,-0.283388629159677,
0.281232202828533));
#32028=CARTESIAN_POINT('Ctrl Pts',(-0.081784357592912,-0.353562500688594,
0.287653104245323));
#32029=CARTESIAN_POINT('Ctrl Pts',(0.0795279050014283,-0.353420115671001,
0.294064881104805));
#32030=CARTESIAN_POINT('Ctrl Pts',(0.24092584464248,-0.275891982678635,
0.301178909350928));
#32031=CARTESIAN_POINT('Ctrl Pts',(0.353854516025502,-0.110325647039583,
0.30899075718887));
#32032=CARTESIAN_POINT('Ctrl Pts',(0.353900252047577,0.107988317536177,
0.317496095092339));
#32033=CARTESIAN_POINT('Ctrl Pts',(0.231000709833199,0.287889843051827,
0.325984040679209));
#32034=CARTESIAN_POINT('Ctrl Pts',(0.028738633598124,0.367371051552907,
0.334454691554125));
#32035=CARTESIAN_POINT('Ctrl Pts',(-0.182879793494325,0.318956105318771,
0.342907496943029));
#32036=CARTESIAN_POINT('Ctrl Pts',(-0.317637558246171,0.173408698249264,
0.35063943767884));
#32037=CARTESIAN_POINT('Ctrl Pts',(-0.356704898032242,0.00120299507430483,
0.357655313472524));
#32038=CARTESIAN_POINT('Ctrl Pts',(-0.321499156165066,-0.153473689430544,
0.36395936824658));
#32039=CARTESIAN_POINT('Ctrl Pts',(-0.222637917146764,-0.277180768652223,
0.370252746171281));
#32040=CARTESIAN_POINT('Ctrl Pts',(-0.0802353799449259,-0.34594748560465,
0.376536355268848));
#32041=CARTESIAN_POINT('Ctrl Pts',(0.0776573488015606,-0.345588985512381,
0.382807725745614));
#32042=CARTESIAN_POINT('Ctrl Pts',(0.219540463198455,-0.277752573568418,
0.389071158618383));
#32043=CARTESIAN_POINT('Ctrl Pts',(0.31776826189951,-0.153592430403837,
0.395318895203019));
#32044=CARTESIAN_POINT('Ctrl Pts',(0.340714022294167,-0.0536225369660789,
0.399484162887714));
#32045=CARTESIAN_POINT('Ctrl Pts',(0.340902966777108,-0.00133151480896985,
0.401559334739322));
#32046=CARTESIAN_POINT('Ctrl Pts',(0.356819906199823,0.000946415613638381,
0.00959378898777047));
#32047=CARTESIAN_POINT('Ctrl Pts',(0.356622877445812,0.0554747871389154,
0.0117577501610062));
#32048=CARTESIAN_POINT('Ctrl Pts',(0.332600183621965,0.16027838517997,0.0161240058481628));
#32049=CARTESIAN_POINT('Ctrl Pts',(0.229891504241292,0.289970795598527,
0.0226522300475058));
#32050=CARTESIAN_POINT('Ctrl Pts',(0.0816316084877276,0.360899492525754,
0.0291986752852052));
#32051=CARTESIAN_POINT('Ctrl Pts',(-0.0832135069240492,0.361230328558343,
0.0357458212344272));
#32052=CARTESIAN_POINT('Ctrl Pts',(-0.231812809233063,0.289476825331103,
0.0423030597446485));
#32053=CARTESIAN_POINT('Ctrl Pts',(-0.334837144696434,0.160482303310326,
0.0488649839626194));
#32054=CARTESIAN_POINT('Ctrl Pts',(-0.365483778755952,0.0261595762945765,
0.0543388585149657));
#32055=CARTESIAN_POINT('Ctrl Pts',(-0.354809005945464,-0.0679232502424184,
0.0581730130440929));
#32056=CARTESIAN_POINT('Ctrl Pts',(-0.33989224429653,-0.119677976039048,
0.060364734388816));
#32057=CARTESIAN_POINT('Ctrl Pts',(-0.302175059373086,-0.210974138360163,
0.0643837854119232));
#32058=CARTESIAN_POINT('Ctrl Pts',(-0.190646477540233,-0.331431753764648,
0.0707818924680168));
#32059=CARTESIAN_POINT('Ctrl Pts',(0.0292333963704387,-0.381494309464949,
0.079566523525864));
#32060=CARTESIAN_POINT('Ctrl Pts',(0.221739847035907,-0.306010819130579,
0.0876276515973482));
#32061=CARTESIAN_POINT('Ctrl Pts',(0.336666969672357,-0.161466621254631,
0.0949624750012229));
#32062=CARTESIAN_POINT('Ctrl Pts',(0.373785362338973,0.00051619079835515,
0.101568677763791));
#32063=CARTESIAN_POINT('Ctrl Pts',(0.336680450911145,0.162727630812525,
0.108179512361388));
#32064=CARTESIAN_POINT('Ctrl Pts',(0.232959901261762,0.292920760014865,
0.114794818884824));
#32065=CARTESIAN_POINT('Ctrl Pts',(0.0828555793888438,0.365149362703125,
0.121414368594224));
#32066=CARTESIAN_POINT('Ctrl Pts',(-0.083865947059046,0.365213561638823,
0.12803802907686));
#32067=CARTESIAN_POINT('Ctrl Pts',(-0.234022832658805,0.292837641030661,
0.134665525254689));
#32068=CARTESIAN_POINT('Ctrl Pts',(-0.33832626279477,0.162301257816034,
0.141296736338365));
#32069=CARTESIAN_POINT('Ctrl Pts',(-0.375003870302502,-0.000208826488397771,
0.147931370051417));
#32070=CARTESIAN_POINT('Ctrl Pts',(-0.326697030597439,-0.218164466286065,
0.156781999918125));
#32071=CARTESIAN_POINT('Ctrl Pts',(-0.0926206709582978,-0.405493959958885,
0.16785291225016));
#32072=CARTESIAN_POINT('Ctrl Pts',(0.25986200463863,-0.325488471750001,
0.181148799941241));
#32073=CARTESIAN_POINT('Ctrl Pts',(0.416506452243591,0.000529987086060091,
0.194453598323448));
#32074=CARTESIAN_POINT('Ctrl Pts',(0.285769963163853,0.271011892920662,
0.205547313860392));
#32075=CARTESIAN_POINT('Ctrl Pts',(0.0834145480806414,0.36692060144113,
0.214424950674681));
#32076=CARTESIAN_POINT('Ctrl Pts',(-0.0838047257248785,0.367335044836678,
0.221084512436662));
#32077=CARTESIAN_POINT('Ctrl Pts',(-0.23494910883256,0.294385829432161,
0.227745038970719));
#32078=CARTESIAN_POINT('Ctrl Pts',(-0.339462559196761,0.163440857085512,
0.234406421306329));
#32079=CARTESIAN_POINT('Ctrl Pts',(-0.376725781361808,-5.13357953542337E-5,
0.241068351157357));
#32080=CARTESIAN_POINT('Ctrl Pts',(-0.33948423973855,-0.163512941907327,
0.247730736309198));
#32081=CARTESIAN_POINT('Ctrl Pts',(-0.234900593046164,-0.29454293296101,
0.254393296337443));
#32082=CARTESIAN_POINT('Ctrl Pts',(-0.0838651541636832,-0.367377563231161,
0.261055777814004));
#32083=CARTESIAN_POINT('Ctrl Pts',(0.0837481144633832,-0.367257140719985,
0.26771807786542));
#32084=CARTESIAN_POINT('Ctrl Pts',(0.251686188309771,-0.286617551856353,
0.275119988445193));
#32085=CARTESIAN_POINT('Ctrl Pts',(0.369425843626467,-0.114101792621121,
0.283261579477833));
#32086=CARTESIAN_POINT('Ctrl Pts',(0.369531467939292,0.113815416132859,
0.292141139676902));
#32087=CARTESIAN_POINT('Ctrl Pts',(0.241042524053221,0.302013576838691,
0.30101906641207));
#32088=CARTESIAN_POINT('Ctrl Pts',(0.0291543790867535,0.385335872444532,
0.309893811897827));
#32089=CARTESIAN_POINT('Ctrl Pts',(-0.192967827991779,0.334584308776725,
0.31876582586576));
#32090=CARTESIAN_POINT('Ctrl Pts',(-0.334683709406543,0.181589938324689,
0.326895446945865));
#32091=CARTESIAN_POINT('Ctrl Pts',(-0.375847011475061,0.000280941035022615,
0.334282274883861));
#32092=CARTESIAN_POINT('Ctrl Pts',(-0.338747168017924,-0.162782317242193,
0.340928662116343));
#32093=CARTESIAN_POINT('Ctrl Pts',(-0.234418175086977,-0.293389546598337,
0.347571447558357));
#32094=CARTESIAN_POINT('Ctrl Pts',(-0.0839196627329805,-0.36605477155107,
0.354213275470552));
#32095=CARTESIAN_POINT('Ctrl Pts',(0.0831384568783626,-0.365745988360452,
0.360847755809616));
#32096=CARTESIAN_POINT('Ctrl Pts',(0.23345413252389,-0.293818325122263,
0.367485688540575));
#32097=CARTESIAN_POINT('Ctrl Pts',(0.337659987033965,-0.162302327276991,
0.374107097871543));
#32098=CARTESIAN_POINT('Ctrl Pts',(0.362055097124151,-0.0558590500639481,
0.378541577281661));
#32099=CARTESIAN_POINT('Ctrl Pts',(0.362254830155579,-0.000582260769330227,
0.380735239452708));
#32100=CARTESIAN_POINT('Ctrl Pts',(0.338971622004564,0.00122203251932272,
0.00102359537366932));
#32101=CARTESIAN_POINT('Ctrl Pts',(0.338783697626477,0.0532307373322113,
0.00308756344638532));
#32102=CARTESIAN_POINT('Ctrl Pts',(0.315964718113649,0.152606406913278,
0.00722828744846333));
#32103=CARTESIAN_POINT('Ctrl Pts',(0.218309382196408,0.276052874201225,
0.0134401453573786));
#32104=CARTESIAN_POINT('Ctrl Pts',(0.0772757052457959,0.343472830879594,
0.0196657590309892));
#32105=CARTESIAN_POINT('Ctrl Pts',(-0.0796437906546839,0.343832157897091,
0.0258990935001355));
#32106=CARTESIAN_POINT('Ctrl Pts',(-0.221168105741207,0.275483129904846,
0.0321436146842611));
#32107=CARTESIAN_POINT('Ctrl Pts',(-0.319355815536309,0.1525741006545,0.0383970939432339));
#32108=CARTESIAN_POINT('Ctrl Pts',(-0.348587348280596,0.024487125389868,
0.0436166583023114));
#32109=CARTESIAN_POINT('Ctrl Pts',(-0.338406476397144,-0.0652656093556688,
0.0472744271625356));
#32110=CARTESIAN_POINT('Ctrl Pts',(-0.324173395788412,-0.114649375725035,
0.0493657286531609));
#32111=CARTESIAN_POINT('Ctrl Pts',(-0.28817943011689,-0.201776041439395,
0.0532012486093371));
#32112=CARTESIAN_POINT('Ctrl Pts',(-0.181699334707641,-0.31681173755523,
0.0593107734350504));
#32113=CARTESIAN_POINT('Ctrl Pts',(0.0284239805984007,-0.364683407763082,
0.067705875653049));
#32114=CARTESIAN_POINT('Ctrl Pts',(0.212569436660183,-0.292507310629878,
0.0754165362004278));
#32115=CARTESIAN_POINT('Ctrl Pts',(0.322599477836521,-0.15414718734826,
0.0824380381498116));
#32116=CARTESIAN_POINT('Ctrl Pts',(0.358168918258642,0.00101965913172981,
0.0887663839950056));
#32117=CARTESIAN_POINT('Ctrl Pts',(0.322612964209937,0.156522586796577,
0.0951037160190564));
#32118=CARTESIAN_POINT('Ctrl Pts',(0.223123755288736,0.281426747319146,
0.10144980766624));
#32119=CARTESIAN_POINT('Ctrl Pts',(0.0790274718456132,0.350779549406656,
0.107804689616852));
#32120=CARTESIAN_POINT('Ctrl Pts',(-0.0811457239354608,0.350856478590949,
0.114168132635694));
#32121=CARTESIAN_POINT('Ctrl Pts',(-0.225519703943384,0.281282412546895,
0.120540137083061));
#32122=CARTESIAN_POINT('Ctrl Pts',(-0.325891610114915,0.155693758731515,
0.126920496791768));
#32123=CARTESIAN_POINT('Ctrl Pts',(-0.36122095909014,-0.000791144434539592,
0.13330915705397));
#32124=CARTESIAN_POINT('Ctrl Pts',(-0.314693637784338,-0.210830847787741,
0.141838312536158));
#32125=CARTESIAN_POINT('Ctrl Pts',(-0.0889149329510122,-0.391648089547769,
0.15251966736754));
#32126=CARTESIAN_POINT('Ctrl Pts',(0.251752009513806,-0.314464296529647,
0.165368610987597));
#32127=CARTESIAN_POINT('Ctrl Pts',(0.403510758968937,0.00106941916421913,
0.178247703836957));
#32128=CARTESIAN_POINT('Ctrl Pts',(0.276843416708589,0.263393027280319,
0.189004268698655));
#32129=CARTESIAN_POINT('Ctrl Pts',(0.0803728550066286,0.356538695494576,
0.197623801156164));
#32130=CARTESIAN_POINT('Ctrl Pts',(-0.082124722949435,0.356960248773731,
0.20409515149567));
#32131=CARTESIAN_POINT('Ctrl Pts',(-0.229138298513218,0.286019839365132,
0.210573278023524));
#32132=CARTESIAN_POINT('Ctrl Pts',(-0.330899321428319,0.158559897907127,
0.217057866538153));
#32133=CARTESIAN_POINT('Ctrl Pts',(-0.367218419527253,-0.00073938524378964,
0.223548897362093));
#32134=CARTESIAN_POINT('Ctrl Pts',(-0.330922063223575,-0.160159900840358,
0.230046159510642));
#32135=CARTESIAN_POINT('Ctrl Pts',(-0.228842222130787,-0.288070568178848,
0.236549534276728));
#32136=CARTESIAN_POINT('Ctrl Pts',(-0.081285433209043,-0.359253201003627,
0.243058873820311));
#32137=CARTESIAN_POINT('Ctrl Pts',(0.0826297065064189,-0.359147357935786,
0.249573876443222));
#32138=CARTESIAN_POINT('Ctrl Pts',(0.247033301398344,-0.280231436867822,
0.256819508059951));
#32139=CARTESIAN_POINT('Ctrl Pts',(0.362424113255112,-0.111212706412119,
0.264796306809896));
#32140=CARTESIAN_POINT('Ctrl Pts',(0.362579145870285,0.112420181971907,
0.273508907247649));
#32141=CARTESIAN_POINT('Ctrl Pts',(0.236388248958002,0.297313675401446,
0.282229310951794));
#32142=CARTESIAN_POINT('Ctrl Pts',(0.0279736069790582,0.379327219628356,
0.290959274341561));
#32143=CARTESIAN_POINT('Ctrl Pts',(-0.190797195609782,0.329377211540027,
0.299696539230122));
#32144=CARTESIAN_POINT('Ctrl Pts',(-0.330585412823941,0.178542452477963,
0.307712637727993));
#32145=CARTESIAN_POINT('Ctrl Pts',(-0.371243104476414,-0.000474749941338493,
0.315006066901667));
#32146=CARTESIAN_POINT('Ctrl Pts',(-0.334606457675173,-0.161629723946379,
0.321573991917603));
#32147=CARTESIAN_POINT('Ctrl Pts',(-0.231407664655513,-0.290837615251207,
0.328145128710479));
#32148=CARTESIAN_POINT('Ctrl Pts',(-0.0823972989864712,-0.362820576105573,
0.334721509538079));
#32149=CARTESIAN_POINT('Ctrl Pts',(0.0831903606930065,-0.362517654622939,
0.341297320706161));
#32150=CARTESIAN_POINT('Ctrl Pts',(0.232343277189241,-0.291185914112765,
0.347883079367717));
#32151=CARTESIAN_POINT('Ctrl Pts',(0.335838209534233,-0.160562321531647,
0.354458910889608));
#32152=CARTESIAN_POINT('Ctrl Pts',(0.360088128449173,-0.0547760251224751,
0.358865946090263));
#32153=CARTESIAN_POINT('Ctrl Pts',(0.360286796917659,0.000206142791657797,
0.361047916196966));
#32154=CARTESIAN_POINT('Ctrl Pts',(0.329995701589468,0.00118959959741402,
0.00102359537366932));
#32155=CARTESIAN_POINT('Ctrl Pts',(0.329812358348379,0.0519304593106012,
0.00303724894968045));
#32156=CARTESIAN_POINT('Ctrl Pts',(0.307603150250096,0.14856309907024,0.007063921474547));
#32157=CARTESIAN_POINT('Ctrl Pts',(0.212522007054295,0.2688270154723,0.0131144005095069));
#32158=CARTESIAN_POINT('Ctrl Pts',(0.0751961041762406,0.33443845631537,
0.0191752186885983));
#32159=CARTESIAN_POINT('Ctrl Pts',(-0.0776142387319525,0.334810528053721,
0.025245738062024));
#32160=CARTESIAN_POINT('Ctrl Pts',(-0.215432226705683,0.268236493442132,
0.0313264548832147));
#32161=CARTESIAN_POINT('Ctrl Pts',(-0.311063582237146,0.148538498980413,
0.0374170400486292));
#32162=CARTESIAN_POINT('Ctrl Pts',(-0.339534702539374,0.0237758430999062,
0.0425008539245673));
#32163=CARTESIAN_POINT('Ctrl Pts',(-0.329617478537296,-0.0636510452603832,
0.0460638560210726));
#32164=CARTESIAN_POINT('Ctrl Pts',(-0.315752180564557,-0.111758567679568,
0.0481010960909614));
#32165=CARTESIAN_POINT('Ctrl Pts',(-0.280687728436729,-0.19663499457563,
0.0518375549362775));
#32166=CARTESIAN_POINT('Ctrl Pts',(-0.176953832876605,-0.308707864139412,
0.0577895429568186));
#32167=CARTESIAN_POINT('Ctrl Pts',(0.0277912542949835,-0.355359243876355,
0.0659698006169508));
#32168=CARTESIAN_POINT('Ctrl Pts',(0.207256209567046,-0.285022432777545,
0.073484386523706));
#32169=CARTESIAN_POINT('Ctrl Pts',(0.31450859302708,-0.150158997366471,
0.0803284879538114));
#32170=CARTESIAN_POINT('Ctrl Pts',(0.349186611535958,0.00111014849211965,
0.0864979120385476));
#32171=CARTESIAN_POINT('Ctrl Pts',(0.314520756767304,0.152731777144028,
0.0926770234710082));
#32172=CARTESIAN_POINT('Ctrl Pts',(0.217500483746742,0.274539465175591,
0.098865768103921));
#32173=CARTESIAN_POINT('Ctrl Pts',(0.0769551264679099,0.342186713109751,
0.105064101576398));
#32174=CARTESIAN_POINT('Ctrl Pts',(-0.0793009475509065,0.342263708237282,
0.111271969453101));
#32175=CARTESIAN_POINT('Ctrl Pts',(-0.220172034550062,0.274381760656883,
0.117489309777858));
#32176=CARTESIAN_POINT('Ctrl Pts',(-0.318128621603507,0.151819046241454,
0.123716067105663));
#32177=CARTESIAN_POINT('Ctrl Pts',(-0.352617648223723,-0.000927697002303161,
0.129952164368648));
#32178=CARTESIAN_POINT('Ctrl Pts',(-0.307197248189229,-0.205991895653557,
0.138279361997572));
#32179=CARTESIAN_POINT('Ctrl Pts',(-0.0867093646975666,-0.382606488631909,
0.148711360096893));
#32180=CARTESIAN_POINT('Ctrl Pts',(0.246157896760925,-0.307226237821677,
0.16126605881999));
#32181=CARTESIAN_POINT('Ctrl Pts',(0.394548713993526,0.00121213976701099,
0.173856329664019));
#32182=CARTESIAN_POINT('Ctrl Pts',(0.270683494680064,0.25779707362797,0.184377360469391));
#32183=CARTESIAN_POINT('Ctrl Pts',(0.0784480660104459,0.348945360245205,
0.192811248605432));
#32184=CARTESIAN_POINT('Ctrl Pts',(-0.0805931042682236,0.349358375490888,
0.199145126960344));
#32185=CARTESIAN_POINT('Ctrl Pts',(-0.224524686851408,0.279914574363962,
0.205487348255157));
#32186=CARTESIAN_POINT('Ctrl Pts',(-0.324178791380424,0.155094279198964,
0.211837815149481));
#32187=CARTESIAN_POINT('Ctrl Pts',(-0.359765231562575,-0.000950160030172512,
0.218196411362682));
#32188=CARTESIAN_POINT('Ctrl Pts',(-0.324199918380757,-0.157162565812712,
0.22456305908972));
#32189=CARTESIAN_POINT('Ctrl Pts',(-0.224151419632265,-0.282543079616346,
0.230937631934188));
#32190=CARTESIAN_POINT('Ctrl Pts',(-0.0794762745603369,-0.352337612459348,
0.237319995378052));
#32191=CARTESIAN_POINT('Ctrl Pts',(0.0812906306420514,-0.352242766117238,
0.243710053380832));
#32192=CARTESIAN_POINT('Ctrl Pts',(0.242583044989387,-0.274824345329341,
0.250818566710242));
#32193=CARTESIAN_POINT('Ctrl Pts',(0.355857692111688,-0.108936398125315,
0.258648506513342));
#32194=CARTESIAN_POINT('Ctrl Pts',(0.35601905515454,0.110643209305051,0.267203260973594));
#32195=CARTESIAN_POINT('Ctrl Pts',(0.232065828412221,0.292295611594562,
0.275770669585301));
#32196=CARTESIAN_POINT('Ctrl Pts',(0.0272435837717024,0.37290401539681,
0.284350408116761));
#32197=CARTESIAN_POINT('Ctrl Pts',(-0.187879927304316,0.323810447294939,
0.292942183858905));
#32198=CARTESIAN_POINT('Ctrl Pts',(-0.325407735789747,0.17542191209667,
0.300828814614272));
#32199=CARTESIAN_POINT('Ctrl Pts',(-0.365431318619722,-0.00075089577638709,
0.308006589851792));
#32200=CARTESIAN_POINT('Ctrl Pts',(-0.329362034481868,-0.159416832712907,
0.314473213303831));
#32201=CARTESIAN_POINT('Ctrl Pts',(-0.227729428899003,-0.286678573326201,
0.320945361203317));
#32202=CARTESIAN_POINT('Ctrl Pts',(-0.0809152203341978,-0.357609127112455,
0.327424927538347));
#32203=CARTESIAN_POINT('Ctrl Pts',(0.0823028008577847,-0.357312684079966,
0.333907107762849));
#32204=CARTESIAN_POINT('Ctrl Pts',(0.229369976399687,-0.286999416296364,
0.340400245782608));
#32205=CARTESIAN_POINT('Ctrl Pts',(0.331477217034357,-0.158117971828307,
0.346888605564388));
#32206=CARTESIAN_POINT('Ctrl Pts',(0.355417803964002,-0.0537733405890617,
0.351235961881927));
#32207=CARTESIAN_POINT('Ctrl Pts',(0.355614008397637,0.000526897379297947,
0.35339086956434));
#32208=CARTESIAN_POINT('',(0.329995701589468,0.00118959959741402,0.00102359537366932));
#32209=CARTESIAN_POINT('Origin',(0.33,2.0618100472869E-19,0.031));
#32210=CARTESIAN_POINT('',(0.355614008397637,0.000526897379297947,0.35339086956434));
#32211=CARTESIAN_POINT('Ctrl Pts',(0.329995701589468,0.00118959959741402,
0.00102359537366932));
#32212=CARTESIAN_POINT('Ctrl Pts',(0.329812358348379,0.0519304593106012,
0.00303724894968045));
#32213=CARTESIAN_POINT('Ctrl Pts',(0.307603150250096,0.14856309907024,0.007063921474547));
#32214=CARTESIAN_POINT('Ctrl Pts',(0.212522007054295,0.2688270154723,0.0131144005095069));
#32215=CARTESIAN_POINT('Ctrl Pts',(0.0751961041762406,0.33443845631537,
0.0191752186885983));
#32216=CARTESIAN_POINT('Ctrl Pts',(-0.0776142387319525,0.334810528053721,
0.025245738062024));
#32217=CARTESIAN_POINT('Ctrl Pts',(-0.215432226705683,0.268236493442132,
0.0313264548832147));
#32218=CARTESIAN_POINT('Ctrl Pts',(-0.311063582237146,0.148538498980413,
0.0374170400486292));
#32219=CARTESIAN_POINT('Ctrl Pts',(-0.339534702539374,0.0237758430999062,
0.0425008539245673));
#32220=CARTESIAN_POINT('Ctrl Pts',(-0.329617478537296,-0.0636510452603832,
0.0460638560210726));
#32221=CARTESIAN_POINT('Ctrl Pts',(-0.315752180564557,-0.111758567679568,
0.0481010960909614));
#32222=CARTESIAN_POINT('Ctrl Pts',(-0.280687728436729,-0.19663499457563,
0.0518375549362775));
#32223=CARTESIAN_POINT('Ctrl Pts',(-0.176953832876605,-0.308707864139412,
0.0577895429568186));
#32224=CARTESIAN_POINT('Ctrl Pts',(0.0277912542949835,-0.355359243876355,
0.0659698006169508));
#32225=CARTESIAN_POINT('Ctrl Pts',(0.207256209567046,-0.285022432777545,
0.073484386523706));
#32226=CARTESIAN_POINT('Ctrl Pts',(0.31450859302708,-0.150158997366471,
0.0803284879538114));
#32227=CARTESIAN_POINT('Ctrl Pts',(0.349186611535958,0.00111014849211965,
0.0864979120385476));
#32228=CARTESIAN_POINT('Ctrl Pts',(0.314520756767304,0.152731777144028,
0.0926770234710082));
#32229=CARTESIAN_POINT('Ctrl Pts',(0.217500483746742,0.274539465175591,
0.098865768103921));
#32230=CARTESIAN_POINT('Ctrl Pts',(0.0769551264679099,0.342186713109751,
0.105064101576398));
#32231=CARTESIAN_POINT('Ctrl Pts',(-0.0793009475509065,0.342263708237282,
0.111271969453101));
#32232=CARTESIAN_POINT('Ctrl Pts',(-0.220172034550062,0.274381760656883,
0.117489309777858));
#32233=CARTESIAN_POINT('Ctrl Pts',(-0.318128621603507,0.151819046241454,
0.123716067105663));
#32234=CARTESIAN_POINT('Ctrl Pts',(-0.352617648223723,-0.000927697002303161,
0.129952164368648));
#32235=CARTESIAN_POINT('Ctrl Pts',(-0.307197248189229,-0.205991895653557,
0.138279361997572));
#32236=CARTESIAN_POINT('Ctrl Pts',(-0.0867093646975666,-0.382606488631909,
0.148711360096893));
#32237=CARTESIAN_POINT('Ctrl Pts',(0.246157896760925,-0.307226237821677,
0.16126605881999));
#32238=CARTESIAN_POINT('Ctrl Pts',(0.394548713993526,0.00121213976701099,
0.173856329664019));
#32239=CARTESIAN_POINT('Ctrl Pts',(0.270683494680064,0.25779707362797,0.184377360469391));
#32240=CARTESIAN_POINT('Ctrl Pts',(0.0784480660104459,0.348945360245205,
0.192811248605432));
#32241=CARTESIAN_POINT('Ctrl Pts',(-0.0805931042682236,0.349358375490888,
0.199145126960344));
#32242=CARTESIAN_POINT('Ctrl Pts',(-0.224524686851408,0.279914574363962,
0.205487348255157));
#32243=CARTESIAN_POINT('Ctrl Pts',(-0.324178791380424,0.155094279198964,
0.211837815149481));
#32244=CARTESIAN_POINT('Ctrl Pts',(-0.359765231562575,-0.000950160030172512,
0.218196411362682));
#32245=CARTESIAN_POINT('Ctrl Pts',(-0.324199918380757,-0.157162565812712,
0.22456305908972));
#32246=CARTESIAN_POINT('Ctrl Pts',(-0.224151419632265,-0.282543079616346,
0.230937631934188));
#32247=CARTESIAN_POINT('Ctrl Pts',(-0.0794762745603369,-0.352337612459348,
0.237319995378052));
#32248=CARTESIAN_POINT('Ctrl Pts',(0.0812906306420514,-0.352242766117238,
0.243710053380832));
#32249=CARTESIAN_POINT('Ctrl Pts',(0.242583044989387,-0.274824345329341,
0.250818566710242));
#32250=CARTESIAN_POINT('Ctrl Pts',(0.355857692111688,-0.108936398125315,
0.258648506513342));
#32251=CARTESIAN_POINT('Ctrl Pts',(0.35601905515454,0.110643209305051,0.267203260973594));
#32252=CARTESIAN_POINT('Ctrl Pts',(0.232065828412221,0.292295611594562,
0.275770669585301));
#32253=CARTESIAN_POINT('Ctrl Pts',(0.0272435837717024,0.37290401539681,
0.284350408116761));
#32254=CARTESIAN_POINT('Ctrl Pts',(-0.187879927304316,0.323810447294939,
0.292942183858905));
#32255=CARTESIAN_POINT('Ctrl Pts',(-0.325407735789747,0.17542191209667,
0.300828814614272));
#32256=CARTESIAN_POINT('Ctrl Pts',(-0.365431318619722,-0.00075089577638709,
0.308006589851792));
#32257=CARTESIAN_POINT('Ctrl Pts',(-0.329362034481868,-0.159416832712907,
0.314473213303831));
#32258=CARTESIAN_POINT('Ctrl Pts',(-0.227729428899003,-0.286678573326201,
0.320945361203317));
#32259=CARTESIAN_POINT('Ctrl Pts',(-0.0809152203341978,-0.357609127112455,
0.327424927538347));
#32260=CARTESIAN_POINT('Ctrl Pts',(0.0823028008577847,-0.357312684079966,
0.333907107762849));
#32261=CARTESIAN_POINT('Ctrl Pts',(0.229369976399687,-0.286999416296364,
0.340400245782608));
#32262=CARTESIAN_POINT('Ctrl Pts',(0.331477217034357,-0.158117971828307,
0.346888605564388));
#32263=CARTESIAN_POINT('Ctrl Pts',(0.355417803964002,-0.0537733405890617,
0.351235961881927));
#32264=CARTESIAN_POINT('Ctrl Pts',(0.355614008397637,0.000526897379297947,
0.35339086956434));
#32265=CARTESIAN_POINT('Origin',(0.33,-3.20923843055709E-16,0.369));
#32266=CARTESIAN_POINT('Origin',(0.33,-3.20923843055709E-16,0.369));
#32267=CARTESIAN_POINT('Origin',(0.33,2.0618100472869E-19,0.031));
#32268=CARTESIAN_POINT('',(0.,0.,0.));
#32269=CARTESIAN_POINT('Origin',(0.,0.,-0.78));
#32270=CARTESIAN_POINT('',(-0.195637724447267,0.00012546577000477,-1.54201303078758));
#32271=CARTESIAN_POINT('',(-0.195587655102992,0.000207352658957182,-1.55218696921242));
#32272=CARTESIAN_POINT('',(-0.1954,-2.39295984553393E-17,-0.78));
#32273=CARTESIAN_POINT('',(0.0862546635467556,0.175513015753855,-1.5646));
#32274=CARTESIAN_POINT('Ctrl Pts',(-0.195637724447267,0.00012546577000477,
-1.54201303078758));
#32275=CARTESIAN_POINT('Ctrl Pts',(-0.195682516033621,0.00666912291098706,
-1.54238744588469));
#32276=CARTESIAN_POINT('Ctrl Pts',(-0.195382767802269,0.0132083530144186,
-1.5427618609818));
#32277=CARTESIAN_POINT('Ctrl Pts',(-0.194724996523875,0.0197110274438995,
-1.54313627607892));
#32278=CARTESIAN_POINT('Ctrl Pts',(-0.188214434300664,0.084073926647727,
-1.54684220375794));
#32279=CARTESIAN_POINT('Ctrl Pts',(-0.146628833277563,0.144855515394664,
-1.55054813143696));
#32280=CARTESIAN_POINT('Ctrl Pts',(-0.0889996456239889,0.174295519526702,
-1.55425405911599));
#32281=CARTESIAN_POINT('Ctrl Pts',(-0.0353713128287438,0.201691677677969,
-1.55770270607733));
#32282=CARTESIAN_POINT('Ctrl Pts',(0.0321503086444766,0.201946916986755,
-1.56115135303866));
#32283=CARTESIAN_POINT('Ctrl Pts',(0.0863567411264609,0.175643900344955,
-1.5646));
#32284=CARTESIAN_POINT('',(-0.0861525859670576,0.175382131162752,-1.5646));
#32285=CARTESIAN_POINT('Origin',(0.,0.,-1.5646));
#32286=CARTESIAN_POINT('Ctrl Pts',(-0.0861525859670577,0.175382131162752,
-1.5646));
#32287=CARTESIAN_POINT('Ctrl Pts',(-0.144492275190264,0.146724051472584,
-1.56089407232098));
#32288=CARTESIAN_POINT('Ctrl Pts',(-0.186904019075789,0.0869180855456786,
-1.55718814464195));
#32289=CARTESIAN_POINT('Ctrl Pts',(-0.194378234588094,0.0227586785356969,
-1.55348221696293));
#32290=CARTESIAN_POINT('Ctrl Pts',(-0.195248998192385,0.015283957422126,
-1.55305046771276));
#32291=CARTESIAN_POINT('Ctrl Pts',(-0.195645561870275,0.00775014794319802,
-1.55261871846259));
#32292=CARTESIAN_POINT('Ctrl Pts',(-0.195587655102992,0.000207352658957182,
-1.55218696921242));
#32293=CARTESIAN_POINT('Origin',(0.,0.,-0.78));
#32294=CARTESIAN_POINT('',(-0.195133752959054,0.000103804320281162,-1.47201303078758));
#32295=CARTESIAN_POINT('',(-0.195118236033235,9.10413472694931E-5,-1.48218696921242));
#32296=CARTESIAN_POINT('',(-0.1954,-2.39295984553393E-17,-0.78));
#32297=CARTESIAN_POINT('Ctrl Pts',(-0.195133752959054,0.000103804320281162,
-1.47201303078758));
#32298=CARTESIAN_POINT('Ctrl Pts',(-0.195258187527039,0.0260059607083059,
-1.47348521314388));
#32299=CARTESIAN_POINT('Ctrl Pts',(-0.190466419891253,0.0518638912152906,
-1.47495739550018));
#32300=CARTESIAN_POINT('Ctrl Pts',(-0.180541931478085,0.0755732040417753,
-1.47642957785648));
#32301=CARTESIAN_POINT('Ctrl Pts',(-0.155558996345714,0.13525670607411,
-1.48013550553551));
#32302=CARTESIAN_POINT('Ctrl Pts',(-0.0980509865883601,0.181324826824306,
-1.48384143321453));
#32303=CARTESIAN_POINT('Ctrl Pts',(-0.0343538193840795,0.192681916213057,
-1.48754736089356));
#32304=CARTESIAN_POINT('Ctrl Pts',(0.0293433478202012,0.204039005601809,
-1.49125328857258));
#32305=CARTESIAN_POINT('Ctrl Pts',(0.0992296724714088,0.180685063629116,
-1.4949592162516));
#32306=CARTESIAN_POINT('Ctrl Pts',(0.143299710901451,0.133312212932569,
-1.49866514393063));
#32307=CARTESIAN_POINT('Ctrl Pts',(0.187369749331493,0.0859393622360219,
-1.50237107160965));
#32308=CARTESIAN_POINT('Ctrl Pts',(0.20562350154037,0.0145476028156198,
-1.50607699928868));
#32309=CARTESIAN_POINT('Ctrl Pts',(0.189702523682121,-0.0481630516398937,
-1.5097829269677));
#32310=CARTESIAN_POINT('Ctrl Pts',(0.173781545823872,-0.110873706095407,
-1.51348885464672));
#32311=CARTESIAN_POINT('Ctrl Pts',(0.123685837898497,-0.164903255586032,
-1.51719478232575));
#32312=CARTESIAN_POINT('Ctrl Pts',(0.0623551946746678,-0.185519277998796,
-1.52090071000477));
#32313=CARTESIAN_POINT('Ctrl Pts',(0.00102455145083888,-0.20613530041156,
-1.5246066376838));
#32314=CARTESIAN_POINT('Ctrl Pts',(-0.0715410270714442,-0.193337795746463,
-1.52831256536282));
#32315=CARTESIAN_POINT('Ctrl Pts',(-0.122106054620926,-0.152966938583555,
-1.53201849304185));
#32316=CARTESIAN_POINT('Ctrl Pts',(-0.167562426162996,-0.116674806024679,
-1.53535000562376));
#32317=CARTESIAN_POINT('Ctrl Pts',(-0.195239172853987,-0.0580994195644015,
-1.53868151820567));
#32318=CARTESIAN_POINT('Ctrl Pts',(-0.195637724447267,0.00012546577000477,
-1.54201303078758));
#32319=CARTESIAN_POINT('Ctrl Pts',(-0.195587655102992,0.000207352658957182,
-1.55218696921242));
#32320=CARTESIAN_POINT('Ctrl Pts',(-0.195148518061644,-0.0569935749705506,
-1.54891279078357));
#32321=CARTESIAN_POINT('Ctrl Pts',(-0.1685728979999,-0.11471127404357,-1.54563861235471));
#32322=CARTESIAN_POINT('Ctrl Pts',(-0.12446534008773,-0.151094701643577,
-1.54236443392585));
#32323=CARTESIAN_POINT('Ctrl Pts',(-0.0745415429359771,-0.19227582671981,
-1.53865850624683));
#32324=CARTESIAN_POINT('Ctrl Pts',(-0.00215726149338587,-0.206125228779217,
-1.53495257856781));
#32325=CARTESIAN_POINT('Ctrl Pts',(0.0594903019840149,-0.186442379139412,
-1.53124665088878));
#32326=CARTESIAN_POINT('Ctrl Pts',(0.121137865461415,-0.166759529499608,
-1.52754072320976));
#32327=CARTESIAN_POINT('Ctrl Pts',(0.172048710973626,-0.113544428160594,
-1.52383479553073));
#32328=CARTESIAN_POINT('Ctrl Pts',(0.188932843502802,-0.0510952853773085,
-1.52012886785171));
#32329=CARTESIAN_POINT('Ctrl Pts',(0.205816976031979,0.0113538574059772,
-1.51642294017269));
#32330=CARTESIAN_POINT('Ctrl Pts',(0.188674395578121,0.0830370416335339,
-1.51271701249366));
#32331=CARTESIAN_POINT('Ctrl Pts',(0.145342587498244,0.131088915832698,
-1.50901108481464));
#32332=CARTESIAN_POINT('Ctrl Pts',(0.102010779418367,0.179140790031861,
-1.50530515713561));
#32333=CARTESIAN_POINT('Ctrl Pts',(0.0324897437124708,0.203561354202632,
-1.50159922945659));
#32334=CARTESIAN_POINT('Ctrl Pts',(-0.0313760153042664,0.193186735136454,
-1.49789330177757));
#32335=CARTESIAN_POINT('Ctrl Pts',(-0.0952417743210041,0.182812116070276,
-1.49418737409854));
#32336=CARTESIAN_POINT('Ctrl Pts',(-0.153452256648582,0.137642313767148,
-1.49048144641952));
#32337=CARTESIAN_POINT('Ctrl Pts',(-0.179353177562788,0.078352807176984,
-1.48677551874049));
#32338=CARTESIAN_POINT('Ctrl Pts',(-0.190043047840084,0.0538827454230738,
-1.48524600223114));
#32339=CARTESIAN_POINT('Ctrl Pts',(-0.195229335108952,0.0270075453386261,
-1.48371648572178));
#32340=CARTESIAN_POINT('Ctrl Pts',(-0.195118236033235,9.10413472694931E-5,
-1.48218696921242));
#32341=CARTESIAN_POINT('Origin',(0.,0.,-0.78));
#32342=CARTESIAN_POINT('',(-0.195261827018658,-0.000164675523070867,-1.40201303078758));
#32343=CARTESIAN_POINT('',(-0.195289109418146,-0.000170586953657092,-1.41218696921242));
#32344=CARTESIAN_POINT('',(-0.1954,-2.39295984553393E-17,-0.78));
#32345=CARTESIAN_POINT('Ctrl Pts',(-0.195261827018658,-0.000164675523070867,
-1.40201303078758));
#32346=CARTESIAN_POINT('Ctrl Pts',(-0.194901371524036,0.0449773888177153,
-1.40458298040307));
#32347=CARTESIAN_POINT('Ctrl Pts',(-0.179326084199164,0.0903439266065276,
-1.40715293001856));
#32348=CARTESIAN_POINT('Ctrl Pts',(-0.150695208685029,0.124890480133385,
-1.40972287963405));
#32349=CARTESIAN_POINT('Ctrl Pts',(-0.109408814040175,0.174707421352147,
-1.41342880731307));
#32350=CARTESIAN_POINT('Ctrl Pts',(-0.0409742153629937,0.202024944228984,
-1.4171347349921));
#32351=CARTESIAN_POINT('Ctrl Pts',(0.0232684964003089,0.194332833555041,
-1.42084066267112));
#32352=CARTESIAN_POINT('Ctrl Pts',(0.0875112081636115,0.186640722881098,
-1.42454659035014));
#32353=CARTESIAN_POINT('Ctrl Pts',(0.147562033013035,0.143938978656375,
-1.42825251802917));
#32354=CARTESIAN_POINT('Ctrl Pts',(0.175920270422902,0.0857830967001064,
-1.43195844570819));
#32355=CARTESIAN_POINT('Ctrl Pts',(0.204278507832768,0.0276272147438382,
-1.43566437338722));
#32356=CARTESIAN_POINT('Ctrl Pts',(0.200944157803076,-0.0459828049439756,
-1.43937030106624));
#32357=CARTESIAN_POINT('Ctrl Pts',(0.167444229718402,-0.101336626764053,
-1.44307622874526));
#32358=CARTESIAN_POINT('Ctrl Pts',(0.133944301633728,-0.15669044858413,
-1.44678215642429));
#32359=CARTESIAN_POINT('Ctrl Pts',(0.0702787954940723,-0.19378807253647,
-1.45048808410331));
#32360=CARTESIAN_POINT('Ctrl Pts',(0.0056037295943023,-0.195640612534423,
-1.45419401178234));
#32361=CARTESIAN_POINT('Ctrl Pts',(-0.0590713363054679,-0.197493152532377,
-1.45789993946136));
#32362=CARTESIAN_POINT('Ctrl Pts',(-0.124755961965352,-0.164100608575943,
-1.46160586714039));
#32363=CARTESIAN_POINT('Ctrl Pts',(-0.1613693445416,-0.110754894940489,
-1.46531179481941));
#32364=CARTESIAN_POINT('Ctrl Pts',(-0.18343803534246,-0.0786008032686692,
-1.46754554014213));
#32365=CARTESIAN_POINT('Ctrl Pts',(-0.194944948132647,-0.0391975909399579,
-1.46977928546485));
#32366=CARTESIAN_POINT('Ctrl Pts',(-0.195133752959054,0.000103804320281162,
-1.47201303078758));
#32367=CARTESIAN_POINT('Ctrl Pts',(-0.195118236033235,9.10413472694931E-5,
-1.48218696921242));
#32368=CARTESIAN_POINT('Ctrl Pts',(-0.194960148645584,-0.038209545522401,
-1.48001055804276));
#32369=CARTESIAN_POINT('Ctrl Pts',(-0.184076125244741,-0.0765937628909216,
-1.47783414687309));
#32370=CARTESIAN_POINT('Ctrl Pts',(-0.163060241772941,-0.108251136057374,
-1.47565773570342));
#32371=CARTESIAN_POINT('Ctrl Pts',(-0.127275025568055,-0.162156361824368,
-1.4719518080244));
#32372=CARTESIAN_POINT('Ctrl Pts',(-0.0621132336574516,-0.196557602481156,
-1.46824588034537));
#32373=CARTESIAN_POINT('Ctrl Pts',(0.00258284575506351,-0.195703428168071,
-1.46453995266635));
#32374=CARTESIAN_POINT('Ctrl Pts',(0.0672789251675789,-0.194849253854986,
-1.46083402498732));
#32375=CARTESIAN_POINT('Ctrl Pts',(0.131509292082006,-0.158739664572028,
-1.4571280973083));
#32376=CARTESIAN_POINT('Ctrl Pts',(0.165859730099399,-0.103909795361192,
-1.45342216962928));
#32377=CARTESIAN_POINT('Ctrl Pts',(0.200210168116792,-0.0490799261503554,
-1.44971624195025));
#32378=CARTESIAN_POINT('Ctrl Pts',(0.204680677237152,0.0244702229883598,
-1.44601031427123));
#32379=CARTESIAN_POINT('Ctrl Pts',(0.177223681968522,0.0830570652693294,
-1.4423043865922));
#32380=CARTESIAN_POINT('Ctrl Pts',(0.149766686699892,0.141643907550299,
-1.43859845891318));
#32381=CARTESIAN_POINT('Ctrl Pts',(0.0903821870422722,0.185267442973523,
-1.43489253123416));
#32382=CARTESIAN_POINT('Ctrl Pts',(0.0262658688812991,0.193950386786294,
-1.43118660355513));
#32383=CARTESIAN_POINT('Ctrl Pts',(-0.037850449279674,0.202633330599066,
-1.42748067587611));
#32384=CARTESIAN_POINT('Ctrl Pts',(-0.106698585944001,0.176375682801386,
-1.42377474819708));
#32385=CARTESIAN_POINT('Ctrl Pts',(-0.14874913778196,0.127202096684771,
-1.42006882051806));
#32386=CARTESIAN_POINT('Ctrl Pts',(-0.178560494578678,0.0923409294319494,
-1.41744153674951));
#32387=CARTESIAN_POINT('Ctrl Pts',(-0.194903459622422,0.0459622751866913,
-1.41481425298097));
#32388=CARTESIAN_POINT('Ctrl Pts',(-0.195289109418146,-0.000170586953657092,
-1.41218696921242));
#32389=CARTESIAN_POINT('Origin',(0.,0.,-0.78));
#32390=CARTESIAN_POINT('',(-0.195719920316492,-1.24737763093352E-5,-1.33201303078758));
#32391=CARTESIAN_POINT('',(-0.195720657836488,6.2470732444266E-6,-1.34218696921242));
#32392=CARTESIAN_POINT('',(-0.1954,-2.39295984553393E-17,-0.78));
#32393=CARTESIAN_POINT('Ctrl Pts',(-0.195719920316492,-1.24737763093352E-5,
-1.33201303078758));
#32394=CARTESIAN_POINT('Ctrl Pts',(-0.195660878792609,0.0640228661772434,
-1.33568074766226));
#32395=CARTESIAN_POINT('Ctrl Pts',(-0.161227285905486,0.128112651091001,
-1.33934846453694));
#32396=CARTESIAN_POINT('Ctrl Pts',(-0.107775864067362,0.163373927248327,
-1.34301618141161));
#32397=CARTESIAN_POINT('Ctrl Pts',(-0.0537675775933861,0.199002560475527,
-1.34672210909064));
#32398=CARTESIAN_POINT('Ctrl Pts',(0.0196568629634197,0.205198876826011,
-1.35042803676966));
#32399=CARTESIAN_POINT('Ctrl Pts',(0.0788722285210952,0.179125231162566,
-1.35413396444869));
#32400=CARTESIAN_POINT('Ctrl Pts',(0.138087594078771,0.15305158549912,-1.35783989212771));
#32401=CARTESIAN_POINT('Ctrl Pts',(0.183093884637317,0.0947079778217447,
-1.36154581980673));
#32402=CARTESIAN_POINT('Ctrl Pts',(0.193280158649522,0.030813264537062,
-1.36525174748576));
#32403=CARTESIAN_POINT('Ctrl Pts',(0.203466432661727,-0.0330814487476208,
-1.36895767516478));
#32404=CARTESIAN_POINT('Ctrl Pts',(0.178832690127592,-0.102527267639611,
-1.37266360284381));
#32405=CARTESIAN_POINT('Ctrl Pts',(0.130660123857593,-0.145720997675018,
-1.37636953052283));
#32406=CARTESIAN_POINT('Ctrl Pts',(0.0824875575875941,-0.188914727710426,
-1.38007545820185));
#32407=CARTESIAN_POINT('Ctrl Pts',(0.0107761675817305,-0.20585636888925,
-1.38378138588088));
#32408=CARTESIAN_POINT('Ctrl Pts',(-0.0516333211096683,-0.188787384501775,
-1.3874873135599));
#32409=CARTESIAN_POINT('Ctrl Pts',(-0.114042809801067,-0.171718400114301,
-1.39119324123893));
#32410=CARTESIAN_POINT('Ctrl Pts',(-0.167150397178,-0.120638790160527,-1.39489916891795));
#32411=CARTESIAN_POINT('Ctrl Pts',(-0.186635095560204,-0.0589408054032964,
-1.39860509659698));
#32412=CARTESIAN_POINT('Ctrl Pts',(-0.192607740429136,-0.0400285212685705,
-1.39974107466051));
#32413=CARTESIAN_POINT('Ctrl Pts',(-0.195421156809523,-0.0201185277405092,
-1.40087705272404));
#32414=CARTESIAN_POINT('Ctrl Pts',(-0.195261827018658,-0.000164675523070867,
-1.40201303078758));
#32415=CARTESIAN_POINT('Ctrl Pts',(-0.195289109418146,-0.000170586953657092,
-1.41218696921242));
#32416=CARTESIAN_POINT('Ctrl Pts',(-0.195447439785316,-0.0191106540360297,
-1.41110832530195));
#32417=CARTESIAN_POINT('Ctrl Pts',(-0.192916081248045,-0.0380092915742028,
-1.41002968139147));
#32418=CARTESIAN_POINT('Ctrl Pts',(-0.1875227974271,-0.0560524670743356,
-1.40895103748099));
#32419=CARTESIAN_POINT('Ctrl Pts',(-0.16899293822269,-0.118043920281279,
-1.40524510980196));
#32420=CARTESIAN_POINT('Ctrl Pts',(-0.116680252802278,-0.169937302259617,
-1.40153918212294));
#32421=CARTESIAN_POINT('Ctrl Pts',(-0.0545417173908017,-0.187967740762588,
-1.39783325444391));
#32422=CARTESIAN_POINT('Ctrl Pts',(0.00759681802067429,-0.205998179265559,
-1.39412732676489));
#32423=CARTESIAN_POINT('Ctrl Pts',(0.0795612034232148,-0.190165674293162,
-1.39042139908587));
#32424=CARTESIAN_POINT('Ctrl Pts',(0.12839486296272,-0.147720799161269,
-1.38671547140684));
#32425=CARTESIAN_POINT('Ctrl Pts',(0.177228522502225,-0.105275924029376,
-1.38300954372782));
#32426=CARTESIAN_POINT('Ctrl Pts',(0.202931456178694,-0.0362186787379851,
-1.37930361604879));
#32427=CARTESIAN_POINT('Ctrl Pts',(0.193732822369028,0.0278256781203122,
-1.37559768836977));
#32428=CARTESIAN_POINT('Ctrl Pts',(0.184534188559362,0.0918700349786089,
-1.37189176069075));
#32429=CARTESIAN_POINT('Ctrl Pts',(0.140433987263561,0.150901503403812,
-1.36818583301172));
#32430=CARTESIAN_POINT('Ctrl Pts',(0.0816282130105867,0.177886223817467,
-1.3644799053327));
#32431=CARTESIAN_POINT('Ctrl Pts',(0.0228224387576129,0.204870944231122,
-1.36077397765367));
#32432=CARTESIAN_POINT('Ctrl Pts',(-0.0506889084525334,0.199808916633229,
-1.35706804997465));
#32433=CARTESIAN_POINT('Ctrl Pts',(-0.105240801513869,0.165018326909214,
-1.35336212229563));
#32434=CARTESIAN_POINT('Ctrl Pts',(-0.159792694575205,0.130227737185199,
-1.3496561946166));
#32435=CARTESIAN_POINT('Ctrl Pts',(-0.19538513348773,0.0657085853350611,
-1.34595026693758));
#32436=CARTESIAN_POINT('Ctrl Pts',(-0.195718314413653,0.00100786455706464,
-1.34224433925855));
#32437=CARTESIAN_POINT('Ctrl Pts',(-0.195720033695728,0.000673995536311298,
-1.34222521590984));
#32438=CARTESIAN_POINT('Ctrl Pts',(-0.195720814104094,0.000340121680791084,
-1.34220609256113));
#32439=CARTESIAN_POINT('Ctrl Pts',(-0.195720657836488,6.2470732444266E-6,
-1.34218696921242));
#32440=CARTESIAN_POINT('Origin',(0.,0.,-0.78));
#32441=CARTESIAN_POINT('',(-0.195298460177798,0.000172226659408109,-1.26201303078758));
#32442=CARTESIAN_POINT('',(-0.195270769970525,0.000166810798610398,-1.27218696921243));
#32443=CARTESIAN_POINT('',(-0.1954,-2.39295984553393E-17,-0.78));
#32444=CARTESIAN_POINT('Ctrl Pts',(-0.195298460177798,0.000172226659408109,
-1.26201303078758));
#32445=CARTESIAN_POINT('Ctrl Pts',(-0.195456041364949,0.018774870840142,
-1.26307258724242));
#32446=CARTESIAN_POINT('Ctrl Pts',(-0.193015100352074,0.0373369952455141,
-1.26413214369726));
#32447=CARTESIAN_POINT('Ctrl Pts',(-0.187808421048084,0.0550878746418882,
-1.26519170015211));
#32448=CARTESIAN_POINT('Ctrl Pts',(-0.16959742638116,0.117173736118483,
-1.26889762783113));
#32449=CARTESIAN_POINT('Ctrl Pts',(-0.117552165740612,0.169335347172546,
-1.27260355551016));
#32450=CARTESIAN_POINT('Ctrl Pts',(-0.0555071253652898,0.187684938084193,
-1.27630948318918));
#32451=CARTESIAN_POINT('Ctrl Pts',(0.00653791501003281,0.206034528995841,
-1.2800154108682));
#32452=CARTESIAN_POINT('Ctrl Pts',(0.07858273512013,0.190572099765074,-1.28372133854723));
#32453=CARTESIAN_POINT('Ctrl Pts',(0.127633912468266,0.148378776567857,
-1.28742726622625));
#32454=CARTESIAN_POINT('Ctrl Pts',(0.176685089816403,0.106185453370639,
-1.29113319390528));
#32455=CARTESIAN_POINT('Ctrl Pts',(0.202742624402578,0.0372612362069706,
-1.2948391215843));
#32456=CARTESIAN_POINT('Ctrl Pts',(0.193873288453785,-0.0268295541039423,
-1.29854504926333));
#32457=CARTESIAN_POINT('Ctrl Pts',(0.185003952504992,-0.0909203444148546,
-1.30225097694235));
#32458=CARTESIAN_POINT('Ctrl Pts',(0.14120774602123,-0.150177707873012,
-1.30595690462137));
#32459=CARTESIAN_POINT('Ctrl Pts',(0.082541443977279,-0.177464325937285,
-1.3096628323004));
#32460=CARTESIAN_POINT('Ctrl Pts',(0.0238751419333269,-0.204750944001557,
-1.31336875997942));
#32461=CARTESIAN_POINT('Ctrl Pts',(-0.0496612556708159,-0.200066816671946,
-1.31707468765845));
#32462=CARTESIAN_POINT('Ctrl Pts',(-0.104391248147666,-0.165557072481202,
-1.32078061533747));
#32463=CARTESIAN_POINT('Ctrl Pts',(-0.159121240624516,-0.131047328290458,
-1.32448654301649));
#32464=CARTESIAN_POINT('Ctrl Pts',(-0.195044827974074,-0.066711967238583,
-1.32819247069552));
#32465=CARTESIAN_POINT('Ctrl Pts',(-0.195710555453279,-0.00201381166068659,
-1.33189839837454));
#32466=CARTESIAN_POINT('Ctrl Pts',(-0.195717419586813,-0.00134672671505401,
-1.33193660917889));
#32467=CARTESIAN_POINT('Ctrl Pts',(-0.195720535419619,-0.000679603200347981,
-1.33197481998323));
#32468=CARTESIAN_POINT('Ctrl Pts',(-0.195719920316492,-1.24737763093352E-5,
-1.33201303078758));
#32469=CARTESIAN_POINT('Ctrl Pts',(-0.195720657836488,6.2470732444266E-6,
-1.34218696921242));
#32470=CARTESIAN_POINT('Ctrl Pts',(-0.195690530890782,-0.0643616817659535,
-1.33850016488211));
#32471=CARTESIAN_POINT('Ctrl Pts',(-0.160845783143528,-0.128757562123285,
-1.33481336055179));
#32472=CARTESIAN_POINT('Ctrl Pts',(-0.106934721662748,-0.163925713548613,
-1.33112655622148));
#32473=CARTESIAN_POINT('Ctrl Pts',(-0.0527440250466008,-0.199276281170437,
-1.32742062854246));
#32474=CARTESIAN_POINT('Ctrl Pts',(0.0207112911250145,-0.205095126708231,
-1.32371470086343));
#32475=CARTESIAN_POINT('Ctrl Pts',(0.0797918581805011,-0.178717469031425,
-1.32000877318441));
#32476=CARTESIAN_POINT('Ctrl Pts',(0.138872425235988,-0.152339811354619,
-1.31630284550538));
#32477=CARTESIAN_POINT('Ctrl Pts',(0.183578243175345,-0.0937656504632113,
-1.31259691782636));
#32478=CARTESIAN_POINT('Ctrl Pts',(0.19343597406848,-0.0298194278652247,
-1.30889099014733));
#32479=CARTESIAN_POINT('Ctrl Pts',(0.203293704961615,0.0341267947327626,
-1.30518506246831));
#32480=CARTESIAN_POINT('Ctrl Pts',(0.178303348808527,0.103445079037329,
-1.30147913478929));
#32481=CARTESIAN_POINT('Ctrl Pts',(0.129909411714146,0.146390638618789,
-1.29777320711026));
#32482=CARTESIAN_POINT('Ctrl Pts',(0.0815154746197661,0.189336198200248,
-1.29406727943124));
#32483=CARTESIAN_POINT('Ctrl Pts',(0.00971795658409383,0.205909033058599,
-1.29036135175221));
#32484=CARTESIAN_POINT('Ctrl Pts',(-0.0526029736186762,0.188519499016706,
-1.28665542407319));
#32485=CARTESIAN_POINT('Ctrl Pts',(-0.114923903821446,0.171129964974812,
-1.28294949639417));
#32486=CARTESIAN_POINT('Ctrl Pts',(-0.167768246191313,0.119778062032674,
-1.27924356871514));
#32487=CARTESIAN_POINT('Ctrl Pts',(-0.186935569481251,0.0579807485361383,
-1.27553764103612));
#32488=CARTESIAN_POINT('Ctrl Pts',(-0.192712207671533,0.039356305477451,
-1.27442075042822));
#32489=CARTESIAN_POINT('Ctrl Pts',(-0.195429975714095,0.0197831099638719,
-1.27330385982032));
#32490=CARTESIAN_POINT('Ctrl Pts',(-0.195270769970525,0.000166810798610398,
-1.27218696921243));
#32491=CARTESIAN_POINT('Origin',(0.,0.,-0.78));
#32492=CARTESIAN_POINT('',(-0.195114271280109,-8.4684676887617E-5,-1.19201303078758));
#32493=CARTESIAN_POINT('',(-0.19512853689889,-9.89862712037332E-5,-1.20218696921242));
#32494=CARTESIAN_POINT('',(-0.1954,-2.39295984553393E-17,-0.78));
#32495=CARTESIAN_POINT('Ctrl Pts',(-0.195114271280109,-8.4684676887617E-5,
-1.19201303078758));
#32496=CARTESIAN_POINT('Ctrl Pts',(-0.194966032011016,0.0378815244295202,
-1.19417035450161));
#32497=CARTESIAN_POINT('Ctrl Pts',(-0.184284351240505,0.0759248070606531,
-1.19632767821564));
#32498=CARTESIAN_POINT('Ctrl Pts',(-0.163614190118679,0.107410771065998,
-1.19848500192967));
#32499=CARTESIAN_POINT('Ctrl Pts',(-0.128106249547212,0.161498483887772,
-1.2021909296087));
#32500=CARTESIAN_POINT('Ctrl Pts',(-0.0631227082835343,0.196235815207334,
-1.20589685728772));
#32501=CARTESIAN_POINT('Ctrl Pts',(0.0015767725456126,0.195714564449213,
-1.20960278496675));
#32502=CARTESIAN_POINT('Ctrl Pts',(0.0662762533747604,0.195193313691093,
-1.21330871264577));
#32503=CARTESIAN_POINT('Ctrl Pts',(0.130691673769378,0.159413480855288,
-1.21701464032479));
#32504=CARTESIAN_POINT('Ctrl Pts',(0.165323547474987,0.104760687280339,
-1.22072056800382));
#32505=CARTESIAN_POINT('Ctrl Pts',(0.199955421180597,0.0501078937053893,
-1.22442649568284));
#32506=CARTESIAN_POINT('Ctrl Pts',(0.204803748197199,-0.0234178606087051,
-1.22813242336187));
#32507=CARTESIAN_POINT('Ctrl Pts',(0.177648203712596,-0.0821449491256642,
-1.23183835104089));
#32508=CARTESIAN_POINT('Ctrl Pts',(0.150492659227993,-0.140872037642623,
-1.23554427871991));
#32509=CARTESIAN_POINT('Ctrl Pts',(0.0913332432421869,-0.184800460362446,
-1.23925020639894));
#32510=CARTESIAN_POINT('Ctrl Pts',(0.0272624185229523,-0.193812892980807,
-1.24295613407796));
#32511=CARTESIAN_POINT('Ctrl Pts',(-0.0368084061962824,-0.202825325599168,
-1.24666206175699));
#32512=CARTESIAN_POINT('Ctrl Pts',(-0.105790639648945,-0.176921768116067,
-1.25036798943601));
#32513=CARTESIAN_POINT('Ctrl Pts',(-0.148093392028626,-0.127964933424953,
-1.25407391711504));
#32514=CARTESIAN_POINT('Ctrl Pts',(-0.178301425292436,-0.0930052769570597,
-1.25672028833922));
#32515=CARTESIAN_POINT('Ctrl Pts',(-0.194904881980768,-0.0462901416537951,
-1.2593666595634));
#32516=CARTESIAN_POINT('Ctrl Pts',(-0.195298460177798,0.000172226659408109,
-1.26201303078758));
#32517=CARTESIAN_POINT('Ctrl Pts',(-0.195270769970525,0.000166810798610398,
-1.27218696921243));
#32518=CARTESIAN_POINT('Ctrl Pts',(-0.194901718991742,-0.0453052572607288,
-1.2695979321413));
#32519=CARTESIAN_POINT('Ctrl Pts',(-0.179073320323297,-0.0910089417293884,
-1.26700889507017));
#32520=CARTESIAN_POINT('Ctrl Pts',(-0.150051297428642,-0.125663369668722,
-1.26441985799905));
#32521=CARTESIAN_POINT('Ctrl Pts',(-0.108509397876086,-0.175267450326114,
-1.26071393032002));
#32522=CARTESIAN_POINT('Ctrl Pts',(-0.0399352945609637,-0.202232887589962,
-1.257008002641));
#32523=CARTESIAN_POINT('Ctrl Pts',(0.0242670287275284,-0.194210673382068,
-1.25330207496197));
#32524=CARTESIAN_POINT('Ctrl Pts',(0.0884693520160203,-0.186188459174174,
-1.24959614728295));
#32525=CARTESIAN_POINT('Ctrl Pts',(0.148299895277882,-0.143178593494537,
-1.24589021960393));
#32526=CARTESIAN_POINT('Ctrl Pts',(0.176358848375927,-0.0848777411188696,
-1.2421842919249));
#32527=CARTESIAN_POINT('Ctrl Pts',(0.204417801473971,-0.0265768887432019,
-1.23847836424588));
#32528=CARTESIAN_POINT('Ctrl Pts',(0.200705164408199,0.0470149503284963,
-1.23477243656685));
#32529=CARTESIAN_POINT('Ctrl Pts',(0.166921164942484,0.102195885592478,
-1.23106650888783));
#32530=CARTESIAN_POINT('Ctrl Pts',(0.13313716547677,0.157376820856459,-1.2273605812088));
#32531=CARTESIAN_POINT('Ctrl Pts',(0.0692818036111139,0.194146852312723,
-1.22365465352978));
#32532=CARTESIAN_POINT('Ctrl Pts',(0.00459808293143662,0.195666890330114,
-1.21994872585076));
#32533=CARTESIAN_POINT('Ctrl Pts',(-0.0600856377482409,0.197186928347506,
-1.21624279817173));
#32534=CARTESIAN_POINT('Ctrl Pts',(-0.125597717241939,0.163456972926025,
-1.21253687049271));
#32535=CARTESIAN_POINT('Ctrl Pts',(-0.161936446693071,0.109923889898341,
-1.20883094281368));
#32536=CARTESIAN_POINT('Ctrl Pts',(-0.183652427151724,0.0779325846854268,
-1.2066162849466));
#32537=CARTESIAN_POINT('Ctrl Pts',(-0.194949895274585,0.0388691013047168,
-1.20440162707951));
#32538=CARTESIAN_POINT('Ctrl Pts',(-0.19512853689889,-9.89862712037332E-5,
-1.20218696921242));
#32539=CARTESIAN_POINT('Origin',(0.,0.,-0.78));
#32540=CARTESIAN_POINT('',(-0.195608501695121,-0.000129687756530023,-1.12201303078758));
#32541=CARTESIAN_POINT('',(-0.195632543296128,-0.000116579743955739,-1.13218696921242));
#32542=CARTESIAN_POINT('',(-0.1954,-2.39295984553393E-17,-0.78));
#32543=CARTESIAN_POINT('Ctrl Pts',(-0.195608501695121,-0.000129687756530023,
-1.12201303078758));
#32544=CARTESIAN_POINT('Ctrl Pts',(-0.195172766225982,0.0567872732702236,
-1.1252681217608));
#32545=CARTESIAN_POINT('Ctrl Pts',(-0.168902158860677,0.114054537459704,
-1.12852321273402));
#32546=CARTESIAN_POINT('Ctrl Pts',(-0.125226675603983,0.150415945518958,
-1.13177830370724));
#32547=CARTESIAN_POINT('Ctrl Pts',(-0.0755020492794521,0.191813482387723,
-1.13548423138626));
#32548=CARTESIAN_POINT('Ctrl Pts',(-0.00321745133242834,0.206113123012647,
-1.13919015906529));
#32549=CARTESIAN_POINT('Ctrl Pts',(0.0585238878228583,0.186766248297933,
-1.14289608674431));
#32550=CARTESIAN_POINT('Ctrl Pts',(0.120265226978144,0.16741937358322,-1.14660201442334));
#32551=CARTESIAN_POINT('Ctrl Pts',(0.171463307341694,0.114425983528869,
-1.15030794210236));
#32552=CARTESIAN_POINT('Ctrl Pts',(0.188671614729629,0.052054766779819,
-1.15401386978138));
#32553=CARTESIAN_POINT('Ctrl Pts',(0.205879922117565,-0.0103164499692322,
-1.15771979746041));
#32554=CARTESIAN_POINT('Ctrl Pts',(0.189098456529886,-0.0820654934129837,
-1.16142572513943));
#32555=CARTESIAN_POINT('Ctrl Pts',(0.146012405929378,-0.13033439401747,
-1.16513165281846));
#32556=CARTESIAN_POINT('Ctrl Pts',(0.10292635532887,-0.178603294621956,
-1.16883758049748));
#32557=CARTESIAN_POINT('Ctrl Pts',(0.0335357197155342,-0.203392052387178,
-1.1725435081765));
#32558=CARTESIAN_POINT('Ctrl Pts',(-0.0303815805162766,-0.193348484645014,
-1.17624943585553));
#32559=CARTESIAN_POINT('Ctrl Pts',(-0.0942988807480878,-0.183304916902849,
-1.17995536353455));
#32560=CARTESIAN_POINT('Ctrl Pts',(-0.152742845598374,-0.138429023653299,
-1.18366129121358));
#32561=CARTESIAN_POINT('Ctrl Pts',(-0.178948658083888,-0.0792720298665307,
-1.1873672188926));
#32562=CARTESIAN_POINT('Ctrl Pts',(-0.189899337275662,-0.0545519697170222,
-1.18891582285759));
#32563=CARTESIAN_POINT('Ctrl Pts',(-0.195220682718685,-0.0273381847313685,
-1.19046442682259));
#32564=CARTESIAN_POINT('Ctrl Pts',(-0.195114271280109,-8.4684676887617E-5,
-1.19201303078758));
#32565=CARTESIAN_POINT('Ctrl Pts',(-0.19512853689889,-9.89862712037332E-5,
-1.20218696921242));
#32566=CARTESIAN_POINT('Ctrl Pts',(-0.195248827651444,-0.026338674800327,
-1.20069569940049));
#32567=CARTESIAN_POINT('Ctrl Pts',(-0.190327637582909,-0.0525351091137002,
-1.19920442958855));
#32568=CARTESIAN_POINT('Ctrl Pts',(-0.180151149975641,-0.0764999183032752,
-1.19771315977661));
#32569=CARTESIAN_POINT('Ctrl Pts',(-0.154861744398516,-0.136054432843319,
-1.19400723209759));
#32570=CARTESIAN_POINT('Ctrl Pts',(-0.0971175538357005,-0.181827251289521,
-1.19030130441856));
#32571=CARTESIAN_POINT('Ctrl Pts',(-0.0333629288067565,-0.192856395588613,
-1.18659537673954));
#32572=CARTESIAN_POINT('Ctrl Pts',(0.0303916962221866,-0.203885539887706,
-1.18288944906052));
#32573=CARTESIAN_POINT('Ctrl Pts',(0.100156755717259,-0.180171010039691,
-1.17918352138149));
#32574=CARTESIAN_POINT('Ctrl Pts',(0.143982859283783,-0.132573038625658,
-1.17547759370247));
#32575=CARTESIAN_POINT('Ctrl Pts',(0.187808962850309,-0.0849750672116236,
-1.17177166602344));
#32576=CARTESIAN_POINT('Ctrl Pts',(0.205696110488285,-0.0134936542315703,
-1.16806573834442));
#32577=CARTESIAN_POINT('Ctrl Pts',(0.189452759510499,0.049135793998185,
-1.16435981066539));
#32578=CARTESIAN_POINT('Ctrl Pts',(0.173209408532712,0.11176524222794,-1.16065388298637));
#32579=CARTESIAN_POINT('Ctrl Pts',(0.122835558939162,0.165542725707396,
-1.15694795530735));
#32580=CARTESIAN_POINT('Ctrl Pts',(0.0614002627451628,0.185840474797084,
-1.15324202762832));
#32581=CARTESIAN_POINT('Ctrl Pts',(-3.50334488365758E-5,0.206138223886772,
-1.1495360999493));
#32582=CARTESIAN_POINT('Ctrl Pts',(-0.0725317762432855,0.192956238586691,
-1.14583017227027));
#32583=CARTESIAN_POINT('Ctrl Pts',(-0.122889582027208,0.152331300024504,
-1.14212424459125));
#32584=CARTESIAN_POINT('Ctrl Pts',(-0.167900298811259,0.116019995837856,
-1.13881181946497));
#32585=CARTESIAN_POINT('Ctrl Pts',(-0.195223980988476,0.0577842214822079,
-1.1354993943387));
#32586=CARTESIAN_POINT('Ctrl Pts',(-0.195632543296128,-0.000116579743955739,
-1.13218696921242));
#32587=CARTESIAN_POINT('Origin',(0.,0.,-0.78));
#32588=CARTESIAN_POINT('',(-0.195514202958888,0.000163480152566932,-1.05201303078758));
#32589=CARTESIAN_POINT('',(-0.195484338171094,0.0001698553111729,-1.06218696921242));
#32590=CARTESIAN_POINT('',(-0.1954,-2.39295984553393E-17,-0.78));
#32591=CARTESIAN_POINT('Ctrl Pts',(-0.195514202958888,0.000163480152566932,
-1.05201303078758));
#32592=CARTESIAN_POINT('Ctrl Pts',(-0.195615708286294,0.0114895985054695,
-1.05265996134096));
#32593=CARTESIAN_POINT('Ctrl Pts',(-0.194716269514434,0.0227996078840509,
-1.05330689189435));
#32594=CARTESIAN_POINT('Ctrl Pts',(-0.192758608403307,0.0339233818421437,
-1.05395382244773));
#32595=CARTESIAN_POINT('Ctrl Pts',(-0.181544189081305,0.0976456803033987,
-1.05765975012676));
#32596=CARTESIAN_POINT('Ctrl Pts',(-0.135603712275178,0.15525657695664,
-1.06136567780578));
#32597=CARTESIAN_POINT('Ctrl Pts',(-0.0759759363407144,0.180372764147859,
-1.0650716054848));
#32598=CARTESIAN_POINT('Ctrl Pts',(-0.0163481604062512,0.205488951339078,
-1.06877753316383));
#32599=CARTESIAN_POINT('Ctrl Pts',(0.0569669146565482,0.198110429068274,
-1.07248346084285));
#32600=CARTESIAN_POINT('Ctrl Pts',(0.110394144327698,0.161616242523277,
-1.07618938852188));
#32601=CARTESIAN_POINT('Ctrl Pts',(0.163821373998849,0.125122055978279,
-1.0798953162009));
#32602=CARTESIAN_POINT('Ctrl Pts',(0.197360758278349,0.0595122051590866,
-1.08360124387992));
#32603=CARTESIAN_POINT('Ctrl Pts',(0.195652704704064,-0.00516682602492472,
-1.08730717155895));
#32604=CARTESIAN_POINT('Ctrl Pts',(0.193944651129778,-0.0698458572089361,
-1.09101309923797));
#32605=CARTESIAN_POINT('Ctrl Pts',(0.156989159701705,-0.133594068757766,
-1.094719026917));
#32606=CARTESIAN_POINT('Ctrl Pts',(0.101710252722787,-0.167217527311745,
-1.09842495459602));
#32607=CARTESIAN_POINT('Ctrl Pts',(0.0464313457438697,-0.200840985865723,
-1.10213088227505));
#32608=CARTESIAN_POINT('Ctrl Pts',(-0.0271709767858934,-0.20433969142485,
-1.10583680995407));
#32609=CARTESIAN_POINT('Ctrl Pts',(-0.0853900233869303,-0.176111387636254,
-1.10954273763309));
#32610=CARTESIAN_POINT('Ctrl Pts',(-0.143609069987967,-0.147883083847658,
-1.11324866531212));
#32611=CARTESIAN_POINT('Ctrl Pts',(-0.186444840660277,-0.0879277707113403,
-1.11695459299114));
#32612=CARTESIAN_POINT('Ctrl Pts',(-0.194280398645414,-0.0237023975868779,
-1.12066052067017));
#32613=CARTESIAN_POINT('Ctrl Pts',(-0.195233616693933,-0.0158891971803149,
-1.12111135737597));
#32614=CARTESIAN_POINT('Ctrl Pts',(-0.195668851941896,-0.0080128023683071,
-1.12156219408177));
#32615=CARTESIAN_POINT('Ctrl Pts',(-0.195608501695121,-0.000129687756530023,
-1.12201303078758));
#32616=CARTESIAN_POINT('Ctrl Pts',(-0.195632543296128,-0.000116579743955739,
-1.13218696921242));
#32617=CARTESIAN_POINT('Ctrl Pts',(-0.19568107882671,-0.00699495803785087,
-1.13179346665968));
#32618=CARTESIAN_POINT('Ctrl Pts',(-0.195349775591712,-0.0138686090342038,
-1.13139996410693));
#32619=CARTESIAN_POINT('Ctrl Pts',(-0.19462316267436,-0.0207002146995433,
-1.13100646155418));
#32620=CARTESIAN_POINT('Ctrl Pts',(-0.187780068764195,-0.0850388990371081,
-1.12730053387515));
#32621=CARTESIAN_POINT('Ctrl Pts',(-0.145875012170469,-0.145648375887944,
-1.12359460619613));
#32622=CARTESIAN_POINT('Ctrl Pts',(-0.0880987027171473,-0.174772117105487,
-1.11988867851711));
#32623=CARTESIAN_POINT('Ctrl Pts',(-0.0303223932638255,-0.20389585832303,
-1.11618275083808));
#32624=CARTESIAN_POINT('Ctrl Pts',(0.0433251690490918,-0.20153386390728,
-1.11247682315906));
#32625=CARTESIAN_POINT('Ctrl Pts',(0.0991165748711698,-0.168767825499369,
-1.10877089548003));
#32626=CARTESIAN_POINT('Ctrl Pts',(0.154907980693247,-0.136001787091459,
-1.10506496780101));
#32627=CARTESIAN_POINT('Ctrl Pts',(0.192843230024486,-0.0728317046913883,
-1.10135904012198));
#32628=CARTESIAN_POINT('Ctrl Pts',(0.195549613669579,-0.00818675342589603,
-1.09765311244296));
#32629=CARTESIAN_POINT('Ctrl Pts',(0.198255997314672,0.0564581978395958,
-1.09394718476394));
#32630=CARTESIAN_POINT('Ctrl Pts',(0.165733515273621,0.122578017970509,
-1.09024125708491));
#32631=CARTESIAN_POINT('Ctrl Pts',(0.112876062611548,0.159892679092233,
-1.08653532940589));
#32632=CARTESIAN_POINT('Ctrl Pts',(0.060018609949475,0.197207340213956,
-1.08282940172686));
#32633=CARTESIAN_POINT('Ctrl Pts',(-0.0131738133336202,0.205716842326488,
-1.07912347404784));
#32634=CARTESIAN_POINT('Ctrl Pts',(-0.0731822319466,0.181524200219397,-1.07541754636881));
#32635=CARTESIAN_POINT('Ctrl Pts',(-0.133190650559579,0.157331558112307,
-1.07171161868979));
#32636=CARTESIAN_POINT('Ctrl Pts',(-0.180015064502443,0.100436771785593,
-1.06800569101077));
#32637=CARTESIAN_POINT('Ctrl Pts',(-0.192211910308214,0.0368952012278665,
-1.06429976333174));
#32638=CARTESIAN_POINT('Ctrl Pts',(-0.194529766665614,0.0248199290122665,
-1.0635954986253));
#32639=CARTESIAN_POINT('Ctrl Pts',(-0.195597076185699,0.012504613517696,
-1.06289123391886));
#32640=CARTESIAN_POINT('Ctrl Pts',(-0.195484338171094,0.0001698553111729,
-1.06218696921242));
#32641=CARTESIAN_POINT('Origin',(0.,0.,-0.78));
#32642=CARTESIAN_POINT('',(-0.195083431151666,3.11826631982926E-5,-0.982013030787577));
#32643=CARTESIAN_POINT('',(-0.19507989431385,1.47260064652817E-5,-0.992186969212424));
#32644=CARTESIAN_POINT('',(-0.1954,-2.39295984553393E-17,-0.78));
#32645=CARTESIAN_POINT('Ctrl Pts',(-0.195083431151666,3.11826631982926E-5,
-0.982013030787577));
#32646=CARTESIAN_POINT('Ctrl Pts',(-0.195127180458594,0.0307478132193151,
-0.98375772860015));
#32647=CARTESIAN_POINT('Ctrl Pts',(-0.188305349657826,0.0614460671203186,
-0.985502426412724));
#32648=CARTESIAN_POINT('Ctrl Pts',(-0.174515300359914,0.0886063591932106,
-0.987247124225297));
#32649=CARTESIAN_POINT('Ctrl Pts',(-0.145223737649203,0.14629776995668,
-0.990953051904321));
#32650=CARTESIAN_POINT('Ctrl Pts',(-0.0844927056335577,0.188026471981535,
-0.994658979583346));
#32651=CARTESIAN_POINT('Ctrl Pts',(-0.0201343994860245,0.194682518235522,
-0.99836490726237));
#32652=CARTESIAN_POINT('Ctrl Pts',(0.0442239066615097,0.201338564489509,
-1.00207083494139));
#32653=CARTESIAN_POINT('Ctrl Pts',(0.112209486940932,0.172921954972627,
-1.00577676262042));
#32654=CARTESIAN_POINT('Ctrl Pts',(0.152687875743341,0.12244627209586,-1.00948269029944));
#32655=CARTESIAN_POINT('Ctrl Pts',(0.19316626454575,0.0719705892190932,
-1.01318861797847));
#32656=CARTESIAN_POINT('Ctrl Pts',(0.206137461871147,-0.000564167017557592,
-1.01689454565749));
#32657=CARTESIAN_POINT('Ctrl Pts',(0.185661218399396,-0.0619402044849644,
-1.02060047333651));
#32658=CARTESIAN_POINT('Ctrl Pts',(0.165184974927645,-0.123316241952371,
-1.02430640101554));
#32659=CARTESIAN_POINT('Ctrl Pts',(0.111261290658746,-0.173533560650533,
-1.02801232869456));
#32660=CARTESIAN_POINT('Ctrl Pts',(0.0485848888924792,-0.189594792967773,
-1.03171825637359));
#32661=CARTESIAN_POINT('Ctrl Pts',(-0.0140915128737879,-0.205656025285014,
-1.03542418405261));
#32662=CARTESIAN_POINT('Ctrl Pts',(-0.0855206321374236,-0.187561171221331,
-1.03913011173164));
#32663=CARTESIAN_POINT('Ctrl Pts',(-0.132991010850304,-0.143596894054857,
-1.04283603941066));
#32664=CARTESIAN_POINT('Ctrl Pts',(-0.172174655166304,-0.107307303665854,
-1.0458950365363));
#32665=CARTESIAN_POINT('Ctrl Pts',(-0.195034237214269,-0.053391825443827,
-1.04895403366194));
#32666=CARTESIAN_POINT('Ctrl Pts',(-0.195514202958888,0.000163480152566932,
-1.05201303078758));
#32667=CARTESIAN_POINT('Ctrl Pts',(-0.195484338171094,0.0001698553111729,
-1.06218696921242));
#32668=CARTESIAN_POINT('Ctrl Pts',(-0.195003834858986,-0.0524024043033798,
-1.05918530623984));
#32669=CARTESIAN_POINT('Ctrl Pts',(-0.173086948518685,-0.105327854283802,
-1.05618364326725));
#32670=CARTESIAN_POINT('Ctrl Pts',(-0.135192047384276,-0.141526621743139,
-1.05318198029467));
#32671=CARTESIAN_POINT('Ctrl Pts',(-0.088406060985887,-0.186218519367677,
-1.04947605261565));
#32672=CARTESIAN_POINT('Ctrl Pts',(-0.0172648105204307,-0.205413959828011,
-1.04577012493662));
#32673=CARTESIAN_POINT('Ctrl Pts',(0.0456520774664714,-0.190322258711306,
-1.0420641972576));
#32674=CARTESIAN_POINT('Ctrl Pts',(0.108568965453373,-0.1752305575946,-1.03835826957857));
#32675=CARTESIAN_POINT('Ctrl Pts',(0.163261490961722,-0.125851714900854,
-1.03465234189955));
#32676=CARTESIAN_POINT('Ctrl Pts',(0.184682834540907,-0.0647991123697999,
-1.03094641422053));
#32677=CARTESIAN_POINT('Ctrl Pts',(0.206104178120092,-0.00374650983874577,
-1.0272404865415));
#32678=CARTESIAN_POINT('Ctrl Pts',(0.194254339770113,0.068979852529617,
-1.02353455886248));
#32679=CARTESIAN_POINT('Ctrl Pts',(0.154560034730616,0.120074435256005,
-1.01982863118345));
#32680=CARTESIAN_POINT('Ctrl Pts',(0.114865729691119,0.171169017982394,
-1.01612270350443));
#32681=CARTESIAN_POINT('Ctrl Pts',(0.0473269579621042,0.200631821066808,
-1.0124167758254));
#32682=CARTESIAN_POINT('Ctrl Pts',(-0.0171264339062948,0.194970150534976,
-1.00871084814638));
#32683=CARTESIAN_POINT('Ctrl Pts',(-0.0815798257746925,0.189308480003144,
-1.00500492046736));
#32684=CARTESIAN_POINT('Ctrl Pts',(-0.142947837782473,0.148522335855069,
-1.00129899278833));
#32685=CARTESIAN_POINT('Ctrl Pts',(-0.173126565373849,0.091290014239414,
-0.997593065109308));
#32686=CARTESIAN_POINT('Ctrl Pts',(-0.187801172250139,0.0634604174552492,
-0.99579103314368));
#32687=CARTESIAN_POINT('Ctrl Pts',(-0.195101212356669,0.0317421955836092,
-0.993989001178052));
#32688=CARTESIAN_POINT('Ctrl Pts',(-0.19507989431385,1.47260064652817E-5,
-0.992186969212424));
#32689=CARTESIAN_POINT('Origin',(0.,0.,-0.78));
#32690=CARTESIAN_POINT('',(-0.195399668261945,-0.000178796749683685,-0.912013030787577));
#32691=CARTESIAN_POINT('',(-0.195430231275111,-0.000177069784595039,-0.922186969212424));
#32692=CARTESIAN_POINT('',(-0.1954,-2.39295984553393E-17,-0.78));
#32693=CARTESIAN_POINT('Ctrl Pts',(-0.195399668261945,-0.000178796749683685,
-0.912013030787577));
#32694=CARTESIAN_POINT('Ctrl Pts',(-0.1949414362207,0.0496606202826749,
-0.914855495859339));
#32695=CARTESIAN_POINT('Ctrl Pts',(-0.175516129708998,0.099817575153293,
-0.917697960931101));
#32696=CARTESIAN_POINT('Ctrl Pts',(-0.141133053901595,0.135602868869345,
-0.920540426002863));
#32697=CARTESIAN_POINT('Ctrl Pts',(-0.0963053465744313,0.182258749288699,
-0.924246353681887));
#32698=CARTESIAN_POINT('Ctrl Pts',(-0.0260520845428951,0.20448535488409,
-0.927952281360912));
#32699=CARTESIAN_POINT('Ctrl Pts',(0.0374537660780799,0.192103858253175,
-0.931658209039936));
#32700=CARTESIAN_POINT('Ctrl Pts',(0.100959616699055,0.17972236162226,-0.93536413671896));
#32701=CARTESIAN_POINT('Ctrl Pts',(0.157718055909468,0.132732762765039,
-0.939070064397983));
#32702=CARTESIAN_POINT('Ctrl Pts',(0.181736164823455,0.0726542727198421,
-0.942775992077008));
#32703=CARTESIAN_POINT('Ctrl Pts',(0.205754273737442,0.0125757826746453,
-0.946481919756032));
#32704=CARTESIAN_POINT('Ctrl Pts',(0.197032052355003,-0.0605915985585276,
-0.950187847435057));
#32705=CARTESIAN_POINT('Ctrl Pts',(0.159563902144046,-0.113340363868098,
-0.953893775114081));
#32706=CARTESIAN_POINT('Ctrl Pts',(0.122095751933089,-0.166089129177668,
-0.957599702793105));
#32707=CARTESIAN_POINT('Ctrl Pts',(0.0558816728936141,-0.198419278563635,
-0.961305630472128));
#32708=CARTESIAN_POINT('Ctrl Pts',(-0.00875514058217604,-0.195524997027423,
-0.965011558151153));
#32709=CARTESIAN_POINT('Ctrl Pts',(-0.0733919540579662,-0.19263071549121,
-0.968717485830177));
#32710=CARTESIAN_POINT('Ctrl Pts',(-0.136451501970072,-0.154512003032818,
-0.972423413509202));
#32711=CARTESIAN_POINT('Ctrl Pts',(-0.169055229223237,-0.0986255870525807,
-0.976129341188226));
#32712=CARTESIAN_POINT('Ctrl Pts',(-0.186309587425756,-0.0690496973854128,
-0.978090571054676));
#32713=CARTESIAN_POINT('Ctrl Pts',(-0.195034252178227,-0.0344976468047085,
-0.980051800921127));
#32714=CARTESIAN_POINT('Ctrl Pts',(-0.195083431151666,3.11826631982926E-5,
-0.982013030787577));
#32715=CARTESIAN_POINT('Ctrl Pts',(-0.19507989431385,1.47260064652817E-5,
-0.992186969212424));
#32716=CARTESIAN_POINT('Ctrl Pts',(-0.195057371222631,-0.0335062072938361,
-0.990283073499028));
#32717=CARTESIAN_POINT('Ctrl Pts',(-0.186862384746915,-0.067037463342061,
-0.988379177785632));
#32718=CARTESIAN_POINT('Ctrl Pts',(-0.17055768636991,-0.0960039059524206,
-0.986475282072236));
#32719=CARTESIAN_POINT('Ctrl Pts',(-0.138820636599626,-0.152387005445362,
-0.982769354393212));
#32720=CARTESIAN_POINT('Ctrl Pts',(-0.0763570938840897,-0.191474705348008,
-0.979063426714187));
#32721=CARTESIAN_POINT('Ctrl Pts',(-0.011772668626182,-0.195366523773639,
-0.975357499035163));
#32722=CARTESIAN_POINT('Ctrl Pts',(0.0528117566317258,-0.19925834219927,
-0.971651571356139));
#32723=CARTESIAN_POINT('Ctrl Pts',(0.119517064432005,-0.167954279147886,
-0.967945643677115));
#32724=CARTESIAN_POINT('Ctrl Pts',(0.157795098781825,-0.115790246300853,
-0.964239715998091));
#32725=CARTESIAN_POINT('Ctrl Pts',(0.196073133131644,-0.0636262134538189,
-0.960533788319067));
#32726=CARTESIAN_POINT('Ctrl Pts',(0.205923894031003,0.00939778918886471,
-0.956827860640042));
#32727=CARTESIAN_POINT('Ctrl Pts',(0.182836157552975,0.0698399157304871,
-0.953121932961018));
#32728=CARTESIAN_POINT('Ctrl Pts',(0.159748421074947,0.13028204227211,-0.949416005281994));
#32729=CARTESIAN_POINT('Ctrl Pts',(0.103722187219531,0.178142292712671,
-0.945710077602971));
#32730=CARTESIAN_POINT('Ctrl Pts',(0.0404150563778447,0.191502735113506,
-0.942004149923947));
#32731=CARTESIAN_POINT('Ctrl Pts',(-0.0228920744638412,0.20486317751434,
-0.938298222244923));
#32732=CARTESIAN_POINT('Ctrl Pts',(-0.0934801022917972,0.183723811875449,
-0.934592294565898));
#32733=CARTESIAN_POINT('Ctrl Pts',(-0.139022752684639,0.137765556558828,
-0.930886366886874));
#32734=CARTESIAN_POINT('Ctrl Pts',(-0.174658780622462,0.101804327769778,
-0.927986567662057));
#32735=CARTESIAN_POINT('Ctrl Pts',(-0.194960310669972,0.0506472724299381,
-0.925086768437241));
#32736=CARTESIAN_POINT('Ctrl Pts',(-0.195430231275111,-0.000177069784595039,
-0.922186969212424));
#32737=CARTESIAN_POINT('Origin',(0.,0.,-0.78));
#32738=CARTESIAN_POINT('',(-0.195686871268044,7.38626216447175E-5,-0.842013030787577));
#32739=CARTESIAN_POINT('',(-0.195669687271611,9.02064299060124E-5,-0.852186969212425));
#32740=CARTESIAN_POINT('',(-0.1954,-2.39295984553393E-17,-0.78));
#32741=CARTESIAN_POINT('Ctrl Pts',(-0.195686871268044,7.38626216447175E-5,
-0.842013030787577));
#32742=CARTESIAN_POINT('Ctrl Pts',(-0.195706672219619,0.00416647744429093,
-0.842247335439503));
#32743=CARTESIAN_POINT('Ctrl Pts',(-0.195589410136118,0.00825793637018049,
-0.84248164009143));
#32744=CARTESIAN_POINT('Ctrl Pts',(-0.195331484399924,0.0123405085514971,
-0.842715944743357));
#32745=CARTESIAN_POINT('Ctrl Pts',(-0.191251948987234,0.0769133504645765,
-0.846421872422381));
#32746=CARTESIAN_POINT('Ctrl Pts',(-0.151982844548713,0.139263011722367,
-0.850127800101405));
#32747=CARTESIAN_POINT('Ctrl Pts',(-0.0955077284300276,0.170836034721377,
-0.853833727780429));
#32748=CARTESIAN_POINT('Ctrl Pts',(-0.0390326123113426,0.202409057720386,
-0.857539655459453));
#32749=CARTESIAN_POINT('Ctrl Pts',(0.0346485154875061,0.203205442460615,
-0.861245583138477));
#32750=CARTESIAN_POINT('Ctrl Pts',(0.0917928740701902,0.172860479054993,
-0.864951510817501));
#32751=CARTESIAN_POINT('Ctrl Pts',(0.148937232652874,0.142515515649371,
-0.868657438496525));
#32752=CARTESIAN_POINT('Ctrl Pts',(0.189544822019393,0.0810292040978983,
-0.872363366175549));
#32753=CARTESIAN_POINT('Ctrl Pts',(0.195019116415376,0.0165596250486992,
-0.876069293854573));
#32754=CARTESIAN_POINT('Ctrl Pts',(0.200493410811359,-0.0479099540005018,
-0.879775221533598));
#32755=CARTESIAN_POINT('Ctrl Pts',(0.170834410236803,-0.11536280054743,
-0.883481149212622));
#32756=CARTESIAN_POINT('Ctrl Pts',(0.11962465866041,-0.154908418071994,
-0.887187076891646));
#32757=CARTESIAN_POINT('Ctrl Pts',(0.0684149070840171,-0.194454035596558,
-0.89089300457067));
#32758=CARTESIAN_POINT('Ctrl Pts',(-0.00434559549421255,-0.206092424098759,
-0.894598932249694));
#32759=CARTESIAN_POINT('Ctrl Pts',(-0.0653356748503108,-0.184493703255807,
-0.898304859928718));
#32760=CARTESIAN_POINT('Ctrl Pts',(-0.126325754206408,-0.162894982412855,
-0.902010787607742));
#32761=CARTESIAN_POINT('Ctrl Pts',(-0.175545410340374,-0.10805915222475,
-0.905716715286767));
#32762=CARTESIAN_POINT('Ctrl Pts',(-0.190454162095962,-0.0450986595090393,
-0.909422642965791));
#32763=CARTESIAN_POINT('Ctrl Pts',(-0.193927826661724,-0.030429179717916,
-0.910286105573053));
#32764=CARTESIAN_POINT('Ctrl Pts',(-0.195538866536356,-0.0153186390656704,
-0.911149568180315));
#32765=CARTESIAN_POINT('Ctrl Pts',(-0.195399668261945,-0.000178796749683685,
-0.912013030787577));
#32766=CARTESIAN_POINT('Ctrl Pts',(-0.195430231275111,-0.000177069784595039,
-0.922186969212424));
#32767=CARTESIAN_POINT('Ctrl Pts',(-0.195560866654202,-0.0143059612177976,
-0.921380840758217));
#32768=CARTESIAN_POINT('Ctrl Pts',(-0.194158895742392,-0.0284091402533054,
-0.920574712304009));
#32769=CARTESIAN_POINT('Ctrl Pts',(-0.191127703969788,-0.0421529964915287,
-0.919768583849801));
#32770=CARTESIAN_POINT('Ctrl Pts',(-0.177192731904368,-0.105336149230912,
-0.916062656170777));
#32771=CARTESIAN_POINT('Ctrl Pts',(-0.1288255148158,-0.160925309715328,
-0.912356728491753));
#32772=CARTESIAN_POINT('Ctrl Pts',(-0.0681761535174188,-0.18346303831984,
-0.908650800812729));
#32773=CARTESIAN_POINT('Ctrl Pts',(-0.00752679221903582,-0.206000766924353,
-0.904944873133705));
#32774=CARTESIAN_POINT('Ctrl Pts',(0.0654047132891616,-0.195487063648961,
-0.901238945454681));
#32775=CARTESIAN_POINT('Ctrl Pts',(0.117218876811456,-0.156736751456187,
-0.897533017775657));
#32776=CARTESIAN_POINT('Ctrl Pts',(0.169033040333749,-0.117986439263414,
-0.893827090096633));
#32777=CARTESIAN_POINT('Ctrl Pts',(0.19972986187014,-0.0509995181532625,
-0.890121162417608));
#32778=CARTESIAN_POINT('Ctrl Pts',(0.195251520181195,0.0135468891229706,
-0.886415234738584));
#32779=CARTESIAN_POINT('Ctrl Pts',(0.190773178492251,0.0780932963992041,
-0.88270930705956));
#32780=CARTESIAN_POINT('Ctrl Pts',(0.15111967357797,0.140199189841518,-0.879003379380536));
#32781=CARTESIAN_POINT('Ctrl Pts',(0.0944506016343666,0.171422746999586,
-0.875297451701512));
#32782=CARTESIAN_POINT('Ctrl Pts',(0.0377815296907636,0.202646304157653,
-0.871591524022488));
#32783=CARTESIAN_POINT('Ctrl Pts',(-0.0359031092821614,0.202987525031474,
-0.867885596343463));
#32784=CARTESIAN_POINT('Ctrl Pts',(-0.0928589264216835,0.172290145167361,
-0.864179668664439));
#32785=CARTESIAN_POINT('Ctrl Pts',(-0.149814743561206,0.141592765303247,
-0.860473740985415));
#32786=CARTESIAN_POINT('Ctrl Pts',(-0.190041738867325,0.079856784701199,
-0.856767813306392));
#32787=CARTESIAN_POINT('Ctrl Pts',(-0.195117682261837,0.0153546216738394,
-0.853061885627368));
#32788=CARTESIAN_POINT('Ctrl Pts',(-0.195517134759009,0.0102786095728853,
-0.852770246822387));
#32789=CARTESIAN_POINT('Ctrl Pts',(-0.195698898966946,0.00518546667535099,
-0.852478608017406));
#32790=CARTESIAN_POINT('Ctrl Pts',(-0.195669687271611,9.02064299060124E-5,
-0.852186969212425));
#32791=CARTESIAN_POINT('Origin',(0.,0.,-0.78));
#32792=CARTESIAN_POINT('',(-0.195179502128291,0.000133953588564106,-0.772013030787577));
#32793=CARTESIAN_POINT('',(-0.195159317916871,0.00012225950549708,-0.782186969212424));
#32794=CARTESIAN_POINT('',(-0.1954,-2.39295984553393E-17,-0.78));
#32795=CARTESIAN_POINT('Ctrl Pts',(-0.195179502128291,0.000133953588564106,
-0.772013030787577));
#32796=CARTESIAN_POINT('Ctrl Pts',(-0.195327243613688,0.0235571326323705,
-0.773345102698692));
#32797=CARTESIAN_POINT('Ctrl Pts',(-0.19142847176856,0.0469327719984332,
-0.774677174609807));
#32798=CARTESIAN_POINT('Ctrl Pts',(-0.183264095800439,0.0687091561557484,
-0.776009246520923));
#32799=CARTESIAN_POINT('Ctrl Pts',(-0.160550166747699,0.129292750873312,
-0.779715174199947));
#32800=CARTESIAN_POINT('Ctrl Pts',(-0.104820645923167,0.177498179312782,
-0.783421101878971));
#32801=CARTESIAN_POINT('Ctrl Pts',(-0.0415972519380625,0.191249432889064,
-0.787127029557995));
#32802=CARTESIAN_POINT('Ctrl Pts',(0.021626142047042,0.205000686465347,
-0.790832957237019));
#32803=CARTESIAN_POINT('Ctrl Pts',(0.0923434091927182,0.184297765178443,
-0.794538884916043));
#32804=CARTESIAN_POINT('Ctrl Pts',(0.138169089040245,0.138621714687765,
-0.798244812595067));
#32805=CARTESIAN_POINT('Ctrl Pts',(0.183994768887772,0.0929456641970873,
-0.801950740274091));
#32806=CARTESIAN_POINT('Ctrl Pts',(0.204928861437148,0.0222964845026362,
-0.805656667953116));
#32807=CARTESIAN_POINT('Ctrl Pts',(0.191384454554165,-0.0409715450549779,
-0.80936259563214));
#32808=CARTESIAN_POINT('Ctrl Pts',(0.177840047671182,-0.104239574612591,
-0.813068523311164));
#32809=CARTESIAN_POINT('Ctrl Pts',(0.129817141355837,-0.160126454033369,
-0.816774450990188));
#32810=CARTESIAN_POINT('Ctrl Pts',(0.069308156927028,-0.183038401251119,
-0.820480378669212));
#32811=CARTESIAN_POINT('Ctrl Pts',(0.00879917249821865,-0.20595034846887,
-0.824186306348236));
#32812=CARTESIAN_POINT('Ctrl Pts',(-0.0641958900440562,-0.195887363483594,
-0.82789223402726));
#32813=CARTESIAN_POINT('Ctrl Pts',(-0.116248438121764,-0.157457859706773,
-0.831598161706284));
#32814=CARTESIAN_POINT('Ctrl Pts',(-0.165010000725506,-0.121458034079663,
-0.835069784733382));
#32815=CARTESIAN_POINT('Ctrl Pts',(-0.19539348639974,-0.060565205969237,
-0.838541407760479));
#32816=CARTESIAN_POINT('Ctrl Pts',(-0.195686871268044,7.38626216447175E-5,
-0.842013030787577));
#32817=CARTESIAN_POINT('Ctrl Pts',(-0.195669687271611,9.02064299060124E-5,
-0.852186969212425));
#32818=CARTESIAN_POINT('Ctrl Pts',(-0.195327698603891,-0.0595612873674038,
-0.848772680338381));
#32819=CARTESIAN_POINT('Ctrl Pts',(-0.166069407350001,-0.119502984320218,
-0.845358391464337));
#32820=CARTESIAN_POINT('Ctrl Pts',(-0.1186654601828,-0.15564441171331,-0.841944102590294));
#32821=CARTESIAN_POINT('Ctrl Pts',(-0.0672124032263472,-0.194872936620427,
-0.83823817491127));
#32822=CARTESIAN_POINT('Ctrl Pts',(0.00561860216946389,-0.206061640981992,
-0.834532247232247));
#32823=CARTESIAN_POINT('Ctrl Pts',(0.0664740945288613,-0.184086580430367,
-0.830826319553223));
#32824=CARTESIAN_POINT('Ctrl Pts',(0.12732958688826,-0.162111519878741,
-0.827120391874198));
#32825=CARTESIAN_POINT('Ctrl Pts',(0.176209566211245,-0.106972694413925,
-0.823414464195174));
#32826=CARTESIAN_POINT('Ctrl Pts',(0.190729108681027,-0.0439213096311892,
-0.81970853651615));
#32827=CARTESIAN_POINT('Ctrl Pts',(0.205248651150809,0.0191300751515466,
-0.816002608837125));
#32828=CARTESIAN_POINT('Ctrl Pts',(0.185407756767386,0.0900940192522011,
-0.812296681158102));
#32829=CARTESIAN_POINT('Ctrl Pts',(0.140292700021491,0.136472094798379,
-0.808590753479078));
#32830=CARTESIAN_POINT('Ctrl Pts',(0.0951776432755965,0.182850170344557,
-0.804884825800054));
#32831=CARTESIAN_POINT('Ctrl Pts',(0.0247884241672289,0.204642377336258,
-0.801178898121029));
#32832=CARTESIAN_POINT('Ctrl Pts',(-0.0386397287071991,0.191868824209177,
-0.797472970442005));
#32833=CARTESIAN_POINT('Ctrl Pts',(-0.102067881581629,0.179095271082094,
-0.793767042762981));
#32834=CARTESIAN_POINT('Ctrl Pts',(-0.15853496822212,0.131755957836228,
-0.790061115083957));
#32835=CARTESIAN_POINT('Ctrl Pts',(-0.182181496662619,0.0715302496273156,
-0.786355187404933));
#32836=CARTESIAN_POINT('Ctrl Pts',(-0.191046923313482,0.0489507576750034,
-0.784965781340764));
#32837=CARTESIAN_POINT('Ctrl Pts',(-0.195299063071233,0.0245599425690687,
-0.783576375276594));
#32838=CARTESIAN_POINT('Ctrl Pts',(-0.195159317916871,0.00012225950549708,
-0.782186969212424));
#32839=CARTESIAN_POINT('Origin',(0.,0.,-0.78));
#32840=CARTESIAN_POINT('',(-0.195201026479454,-0.00014426443444554,-0.702013030787577));
#32841=CARTESIAN_POINT('',(-0.195224781921234,-0.000153591798034323,-0.712186969212424));
#32842=CARTESIAN_POINT('',(-0.1954,-2.39295984553393E-17,-0.78));
#32843=CARTESIAN_POINT('Ctrl Pts',(-0.195201026479454,-0.00014426443444554,
-0.702013030787577));
#32844=CARTESIAN_POINT('Ctrl Pts',(-0.194908728495298,0.0425702348016472,
-0.704442869957881));
#32845=CARTESIAN_POINT('Ctrl Pts',(-0.181117466392626,0.0854564354592731,
-0.706872709128184));
#32846=CARTESIAN_POINT('Ctrl Pts',(-0.155298824010949,0.119117388361245,
-0.709302548298488));
#32847=CARTESIAN_POINT('Ctrl Pts',(-0.11592090031688,0.170456200652327,
-0.713008475977512));
#32848=CARTESIAN_POINT('Ctrl Pts',(-0.0485654147671141,0.200335648249632,
-0.716714403656536));
#32849=CARTESIAN_POINT('Ctrl Pts',(0.0159217232587258,0.195072231949245,
-0.720420331335561));
#32850=CARTESIAN_POINT('Ctrl Pts',(0.0804088612845667,0.189808815648857,
-0.724126259014585));
#32851=CARTESIAN_POINT('Ctrl Pts',(0.142027651786483,0.149402535450774,
-0.727832186693609));
#32852=CARTESIAN_POINT('Ctrl Pts',(0.172559344466851,0.0923577261865951,
-0.731538114372633));
#32853=CARTESIAN_POINT('Ctrl Pts',(0.203091037147218,0.0353129169224173,
-0.735244042051657));
#32854=CARTESIAN_POINT('Ctrl Pts',(0.202535632006039,-0.0383704214078547,
-0.738949969730681));
#32855=CARTESIAN_POINT('Ctrl Pts',(0.171147480660172,-0.0949484955797788,
-0.742655897409705));
#32856=CARTESIAN_POINT('Ctrl Pts',(0.139759329314305,-0.151526569751704,
-0.746361825088729));
#32857=CARTESIAN_POINT('Ctrl Pts',(0.0775384317637469,-0.190999379765278,
-0.750067752767754));
#32858=CARTESIAN_POINT('Ctrl Pts',(0.0129792773837577,-0.195290079901112,
-0.753773680446778));
#32859=CARTESIAN_POINT('Ctrl Pts',(-0.0515798769962315,-0.199580780036946,
-0.757479608125802));
#32860=CARTESIAN_POINT('Ctrl Pts',(-0.118477288205653,-0.16868937029504,
-0.761185535804826));
#32861=CARTESIAN_POINT('Ctrl Pts',(-0.157076825169889,-0.116762784926257,
-0.76489146348385));
#32862=CARTESIAN_POINT('Ctrl Pts',(-0.181802006392339,-0.0835008772848329,
-0.767265319251759));
#32863=CARTESIAN_POINT('Ctrl Pts',(-0.194916215308456,-0.041607973564115,
-0.769639175019668));
#32864=CARTESIAN_POINT('Ctrl Pts',(-0.195179502128291,0.000133953588564106,
-0.772013030787577));
#32865=CARTESIAN_POINT('Ctrl Pts',(-0.195159317916871,0.00012225950549708,
-0.782186969212424));
#32866=CARTESIAN_POINT('Ctrl Pts',(-0.194926324352933,-0.0406220718268677,
-0.77987044759757));
#32867=CARTESIAN_POINT('Ctrl Pts',(-0.182484747099273,-0.0814966869427612,
-0.777553925982715));
#32868=CARTESIAN_POINT('Ctrl Pts',(-0.158860717615929,-0.114323867746546,
-0.77523740436786));
#32869=CARTESIAN_POINT('Ctrl Pts',(-0.121067439888232,-0.166840173739539,
-0.771531476688836));
#32870=CARTESIAN_POINT('Ctrl Pts',(-0.0546549141923333,-0.198760682553565,
-0.767825549009812));
#32871=CARTESIAN_POINT('Ctrl Pts',(0.00996278506392166,-0.195467176916607,
-0.764119621330788));
#32872=CARTESIAN_POINT('Ctrl Pts',(0.0745804843201748,-0.192173671279648,
-0.760413693651764));
#32873=CARTESIAN_POINT('Ctrl Pts',(0.137403357136784,-0.153666151191704,
-0.75670776597274));
#32874=CARTESIAN_POINT('Ctrl Pts',(0.169661235411597,-0.0975794011899468,
-0.753001838293716));
#32875=CARTESIAN_POINT('Ctrl Pts',(0.201919113686411,-0.0414926511881883,
-0.749295910614691));
#32876=CARTESIAN_POINT('Ctrl Pts',(0.20361199741943,0.0321733287273828,
-0.745589982935668));
#32877=CARTESIAN_POINT('Ctrl Pts',(0.173964618823738,0.0896826947381129,
-0.741884055256643));
#32878=CARTESIAN_POINT('Ctrl Pts',(0.144317240228045,0.147192060748842,
-0.738178127577619));
#32879=CARTESIAN_POINT('Ctrl Pts',(0.0833295993036407,0.188544812854729,
-0.734472199898595));
#32880=CARTESIAN_POINT('Ctrl Pts',(0.0189314070440128,0.194803172883071,
-0.73076627221957));
#32881=CARTESIAN_POINT('Ctrl Pts',(-0.0454667852156141,0.201061532911413,
-0.727060344540546));
#32882=CARTESIAN_POINT('Ctrl Pts',(-0.113275528810465,0.172225500862211,
-0.723354416861523));
#32883=CARTESIAN_POINT('Ctrl Pts',(-0.153441341711563,0.121500736589262,
-0.719648489182499));
#32884=CARTESIAN_POINT('Ctrl Pts',(-0.180397976328058,0.087457632821372,
-0.717161315859141));
#32885=CARTESIAN_POINT('Ctrl Pts',(-0.194903666161545,0.043555393663416,
-0.714674142535782));
#32886=CARTESIAN_POINT('Ctrl Pts',(-0.195224781921234,-0.000153591798034323,
-0.712186969212424));
#32887=CARTESIAN_POINT('Origin',(0.,0.,-0.78));
#32888=CARTESIAN_POINT('',(-0.195700638108693,-5.70533469873291E-5,-0.632013030787577));
#32889=CARTESIAN_POINT('',(-0.195711310405279,-3.91468106102235E-5,-0.642186969212423));
#32890=CARTESIAN_POINT('',(-0.1954,-2.39295984553393E-17,-0.78));
#32891=CARTESIAN_POINT('Ctrl Pts',(-0.195700638108693,-5.70533469873291E-5,
-0.632013030787577));
#32892=CARTESIAN_POINT('Ctrl Pts',(-0.195463028848959,0.0615483382290371,
-0.635540637217069));
#32893=CARTESIAN_POINT('Ctrl Pts',(-0.163955310161744,0.123363079763,-0.639068243646561));
#32894=CARTESIAN_POINT('Ctrl Pts',(-0.113861614071831,0.159192367248385,
-0.642595850076054));
#32895=CARTESIAN_POINT('Ctrl Pts',(-0.0612356710720203,0.196832832778126,
-0.646301777755078));
#32896=CARTESIAN_POINT('Ctrl Pts',(0.0119027926823546,0.205794302636062,
-0.650007705434102));
#32897=CARTESIAN_POINT('Ctrl Pts',(0.0720595130386693,0.181972809864049,
-0.653713633113126));
#32898=CARTESIAN_POINT('Ctrl Pts',(0.132216233394983,0.158151317092035,
-0.65741956079215));
#32899=CARTESIAN_POINT('Ctrl Pts',(0.179391210353237,0.101546861690073,
-0.661125488471174));
#32900=CARTESIAN_POINT('Ctrl Pts',(0.191980337694572,0.0380818445964134,
-0.664831416150198));
#32901=CARTESIAN_POINT('Ctrl Pts',(0.204569465035907,-0.0253831724972469,
-0.668537343829222));
#32902=CARTESIAN_POINT('Ctrl Pts',(0.182572742760322,-0.0957087512826043,
-0.672243271508247));
#32903=CARTESIAN_POINT('Ctrl Pts',(0.136063721617594,-0.140688807688307,
-0.675949199187271));
#32904=CARTESIAN_POINT('Ctrl Pts',(0.0895547004748648,-0.185668864094009,
-0.679655126866295));
#32905=CARTESIAN_POINT('Ctrl Pts',(0.0185333804649922,-0.205303398120056,
-0.683361054545319));
#32906=CARTESIAN_POINT('Ctrl Pts',(-0.0444755348460918,-0.190600639425322,
-0.687066982224343));
#32907=CARTESIAN_POINT('Ctrl Pts',(-0.107484450157176,-0.175897880730587,
-0.690772909903367));
#32908=CARTESIAN_POINT('Ctrl Pts',(-0.162480960769471,-0.126857829315072,
-0.694478837582392));
#32909=CARTESIAN_POINT('Ctrl Pts',(-0.184279035156432,-0.0659387151148841,
-0.698184765261416));
#32910=CARTESIAN_POINT('Ctrl Pts',(-0.191784921575877,-0.044962002041856,
-0.699460853770136));
#32911=CARTESIAN_POINT('Ctrl Pts',(-0.195354533799305,-0.0225768115334816,
-0.700736942278857));
#32912=CARTESIAN_POINT('Ctrl Pts',(-0.195201026479454,-0.00014426443444554,
-0.702013030787577));
#32913=CARTESIAN_POINT('Ctrl Pts',(-0.195224781921234,-0.000153591798034323,
-0.712186969212424));
#32914=CARTESIAN_POINT('Ctrl Pts',(-0.195382133733879,-0.0215716875586284,
-0.710968214856758));
#32915=CARTESIAN_POINT('Ctrl Pts',(-0.192133548947981,-0.0429433801044127,
-0.709749460501092));
#32916=CARTESIAN_POINT('Ctrl Pts',(-0.185275048015275,-0.0630859011262851,
-0.708530706145426));
#32917=CARTESIAN_POINT('Ctrl Pts',(-0.164420059210545,-0.124334278072184,
-0.704824778466402));
#32918=CARTESIAN_POINT('Ctrl Pts',(-0.11018719939374,-0.174217535467284,
-0.701118850787378));
#32919=CARTESIAN_POINT('Ctrl Pts',(-0.0474127809402028,-0.189891291378763,
-0.697412923108353));
#32920=CARTESIAN_POINT('Ctrl Pts',(0.0153616375133333,-0.205565047290241,
-0.693706995429329));
#32921=CARTESIAN_POINT('Ctrl Pts',(0.0866776146036013,-0.187029301718099,
-0.690001067750306));
#32922=CARTESIAN_POINT('Ctrl Pts',(0.133875506521484,-0.142772627249042,
-0.686295140071282));
#32923=CARTESIAN_POINT('Ctrl Pts',(0.181073398439368,-0.0985159527799843,
-0.682589212392258));
#32924=CARTESIAN_POINT('Ctrl Pts',(0.204153205184866,-0.0285383494140109,
-0.678883284713233));
#32925=CARTESIAN_POINT('Ctrl Pts',(0.192545370001613,0.0351134565219624,
-0.675177357034209));
#32926=CARTESIAN_POINT('Ctrl Pts',(0.18093753481836,0.0987652624579367,
-0.671471429355185));
#32927=CARTESIAN_POINT('Ctrl Pts',(0.134642057706355,0.156091270963911,
-0.66776550167616));
#32928=CARTESIAN_POINT('Ctrl Pts',(0.0748602718610678,0.180838640878726,
-0.664059573997136));
#32929=CARTESIAN_POINT('Ctrl Pts',(0.0150784860157823,0.205586010793541,
-0.660353646318112));
#32930=CARTESIAN_POINT('Ctrl Pts',(-0.0581896085627842,0.197754742117199,
-0.656647718639089));
#32931=CARTESIAN_POINT('Ctrl Pts',(-0.11139038239158,0.160931218378025,
-0.652941790960065));
#32932=CARTESIAN_POINT('Ctrl Pts',(-0.162854315214999,0.125309868994405,
-0.649356850377518));
#32933=CARTESIAN_POINT('Ctrl Pts',(-0.195539811246121,0.0625583792222248,
-0.64577190979497));
#32934=CARTESIAN_POINT('Ctrl Pts',(-0.195711310405279,-3.91468106102235E-5,
-0.642186969212423));
#32935=CARTESIAN_POINT('Origin',(0.,0.,-0.78));
#32936=CARTESIAN_POINT('',(-0.195370054518654,0.000178868712723643,-0.562013030787577));
#32937=CARTESIAN_POINT('',(-0.195340204128639,0.000177311515467854,-0.572186969212424));
#32938=CARTESIAN_POINT('',(-0.1954,-2.39295984553393E-17,-0.78));
#32939=CARTESIAN_POINT('Ctrl Pts',(-0.195370054518654,0.000178868712723643,
-0.562013030787577));
#32940=CARTESIAN_POINT('Ctrl Pts',(-0.195516344455089,0.0163065574472149,
-0.562932476797233));
#32941=CARTESIAN_POINT('Ctrl Pts',(-0.193686613410829,0.0324015011250242,
-0.56385192280689));
#32942=CARTESIAN_POINT('Ctrl Pts',(-0.189752676663686,0.047964556165507,
-0.564771368816547));
#32943=CARTESIAN_POINT('Ctrl Pts',(-0.173896514446821,0.110693151253132,
-0.568477296495571));
#32944=CARTESIAN_POINT('Ctrl Pts',(-0.123855822614536,0.164780783696336,
-0.572183224174595));
#32945=CARTESIAN_POINT('Ctrl Pts',(-0.0625470812865084,0.185457648997625,
-0.575889151853619));
#32946=CARTESIAN_POINT('Ctrl Pts',(-0.00123833995847777,0.206134514298915,
-0.579595079532643));
#32947=CARTESIAN_POINT('Ctrl Pts',(0.0713384508652961,0.193400612458291,
-0.583301007211667));
#32948=CARTESIAN_POINT('Ctrl Pts',(0.121946249026466,0.153087521691229,
-0.587006934890692));
#32949=CARTESIAN_POINT('Ctrl Pts',(0.172554047187635,0.112774430924167,
-0.590712862569716));
#32950=CARTESIAN_POINT('Ctrl Pts',(0.201192852686197,0.0448821512306687,
-0.59441879024874));
#32951=CARTESIAN_POINT('Ctrl Pts',(0.194747326928141,-0.0194975794274909,
-0.598124717927764));
#32952=CARTESIAN_POINT('Ctrl Pts',(0.188301801170084,-0.0838773100856497,
-0.601830645606789));
#32953=CARTESIAN_POINT('Ctrl Pts',(0.146771944155409,-0.144744491708471,
-0.605536573285813));
#32954=CARTESIAN_POINT('Ctrl Pts',(0.0891766404718725,-0.174224578470828,
-0.609242500964837));
#32955=CARTESIAN_POINT('Ctrl Pts',(0.0315813367883353,-0.203704665233185,
-0.61294842864386));
#32956=CARTESIAN_POINT('Ctrl Pts',(-0.0420794135640636,-0.201797657135079,
-0.616654356322884));
#32957=CARTESIAN_POINT('Ctrl Pts',(-0.0980721616812089,-0.169376881693938,
-0.620360284001909));
#32958=CARTESIAN_POINT('Ctrl Pts',(-0.154064909798354,-0.136956106252797,
-0.624066211680933));
#32959=CARTESIAN_POINT('Ctrl Pts',(-0.192389655680245,-0.0740215634686213,
-0.627772139359957));
#32960=CARTESIAN_POINT('Ctrl Pts',(-0.195495317498567,-0.00939456147576089,
-0.631478067038982));
#32961=CARTESIAN_POINT('Ctrl Pts',(-0.19564475524912,-0.00628484948270523,
-0.631656388288513));
#32962=CARTESIAN_POINT('Ctrl Pts',(-0.195712649306921,-0.00317121889331525,
-0.631834709538045));
#32963=CARTESIAN_POINT('Ctrl Pts',(-0.195700638108693,-5.70533469873291E-5,
-0.632013030787577));
#32964=CARTESIAN_POINT('Ctrl Pts',(-0.195711310405279,-3.91468106102235E-5,
-0.642186969212423));
#32965=CARTESIAN_POINT('Ctrl Pts',(-0.195717098279537,-0.00215173215114592,
-0.642065982115946));
#32966=CARTESIAN_POINT('Ctrl Pts',(-0.195685853524789,-0.00426414213083437,
-0.641944995019469));
#32967=CARTESIAN_POINT('Ctrl Pts',(-0.195617048160817,-0.00637532797793774,
-0.641824007922991));
#32968=CARTESIAN_POINT('Ctrl Pts',(-0.193509487022232,-0.0710425717927132,
-0.638118080243967));
#32969=CARTESIAN_POINT('Ctrl Pts',(-0.156160911666037,-0.134561280620253,
-0.634412152564944));
#32970=CARTESIAN_POINT('Ctrl Pts',(-0.100675359892449,-0.167842623455736,
-0.63070622488592));
#32971=CARTESIAN_POINT('Ctrl Pts',(-0.0451898081188624,-0.201123966291216,
-0.627000297206896));
#32972=CARTESIAN_POINT('Ctrl Pts',(0.0284327200721153,-0.204167943134643,
-0.623294369527871));
#32973=CARTESIAN_POINT('Ctrl Pts',(0.0864762798789366,-0.175580543786257,
-0.619588441848847));
#32974=CARTESIAN_POINT('Ctrl Pts',(0.14451983968576,-0.14699314443787,-0.615882514169823));
#32975=CARTESIAN_POINT('Ctrl Pts',(0.186984431108425,-0.0867743688976694,
-0.612176586490799));
#32976=CARTESIAN_POINT('Ctrl Pts',(0.194423101487104,-0.0225018209510558,
-0.608470658811775));
#32977=CARTESIAN_POINT('Ctrl Pts',(0.201861771865782,0.0417707269955578,
-0.604764731132751));
#32978=CARTESIAN_POINT('Ctrl Pts',(0.174274521200472,0.110097047348584,
-0.601058803453726));
#32979=CARTESIAN_POINT('Ctrl Pts',(0.12429512129327,0.151186630231212,-0.597352875774702));
#32980=CARTESIAN_POINT('Ctrl Pts',(0.0743157213860675,0.19227621311384,
-0.593646948095678));
#32981=CARTESIAN_POINT('Ctrl Pts',(0.00194417223697229,0.206129058526068,
-0.589941020416654));
#32982=CARTESIAN_POINT('Ctrl Pts',(-0.0596764758368093,0.186401160322774,
-0.58623509273763));
#32983=CARTESIAN_POINT('Ctrl Pts',(-0.121297123910592,0.16667326211948,
-0.582529165058606));
#32984=CARTESIAN_POINT('Ctrl Pts',(-0.17216687090906,0.113364620300662,
-0.578823237379581));
#32985=CARTESIAN_POINT('Ctrl Pts',(-0.188989565178469,0.0508882952321173,
-0.575117309700557));
#32986=CARTESIAN_POINT('Ctrl Pts',(-0.193423562673541,0.0344212618057884,
-0.574140529537846));
#32987=CARTESIAN_POINT('Ctrl Pts',(-0.195492297890079,0.0173173457821699,
-0.573163749375135));
#32988=CARTESIAN_POINT('Ctrl Pts',(-0.195340204128639,0.000177311515467854,
-0.572186969212424));
#32989=CARTESIAN_POINT('Origin',(0.,0.,-0.78));
#32990=CARTESIAN_POINT('',(-0.195089308542836,-4.70021948510008E-5,-0.492013030787576));
#32991=CARTESIAN_POINT('',(-0.195097772416105,-6.2815082009945E-5,-0.502186969212424));
#32992=CARTESIAN_POINT('',(-0.1954,-2.39295984553393E-17,-0.78));
#32993=CARTESIAN_POINT('Ctrl Pts',(-0.195089308542836,-4.70021948510008E-5,
-0.492013030787576));
#32994=CARTESIAN_POINT('Ctrl Pts',(-0.195012935367883,0.0354647848324114,
-0.494030244056422));
#32995=CARTESIAN_POINT('Ctrl Pts',(-0.185752717710553,0.0710136700588578,
-0.496047457325267));
#32996=CARTESIAN_POINT('Ctrl Pts',(-0.167549278060548,0.101162821088464,
-0.498064670594113));
#32997=CARTESIAN_POINT('Ctrl Pts',(-0.134106789904096,0.156551398501326,
-0.501770598273137));
#32998=CARTESIAN_POINT('Ctrl Pts',(-0.0704797828327725,0.193715181859728,
-0.505476525952161));
#32999=CARTESIAN_POINT('Ctrl Pts',(-0.00580668377942445,0.195634760133963,
-0.509182453631185));
#33000=CARTESIAN_POINT('Ctrl Pts',(0.0588664152739227,0.197554338408197,
-0.512888381310209));
#33001=CARTESIAN_POINT('Ctrl Pts',(0.124585606309294,0.164229711598261,
-0.516594308989234));
#33002=CARTESIAN_POINT('Ctrl Pts',(0.161254332310831,0.110922122501218,
-0.520300236668258));
#33003=CARTESIAN_POINT('Ctrl Pts',(0.197923058312368,0.0576145334041769,
-0.524006164347282));
#33004=CARTESIAN_POINT('Ctrl Pts',(0.205541319280075,-0.0156760179799715,
-0.527712092026305));
#33005=CARTESIAN_POINT('Ctrl Pts',(0.180620280035612,-0.0753856179190998,
-0.53141801970533));
#33006=CARTESIAN_POINT('Ctrl Pts',(0.155699240791148,-0.135095217858229,
-0.535123947384354));
#33007=CARTESIAN_POINT('Ctrl Pts',(0.0982389013345159,-0.181223866352336,
-0.538829875063378));
#33008=CARTESIAN_POINT('Ctrl Pts',(0.0345536206126452,-0.192646630522687,
-0.542535802742402));
#33009=CARTESIAN_POINT('Ctrl Pts',(-0.0291316601092254,-0.204069394693038,
-0.546241730421427));
#33010=CARTESIAN_POINT('Ctrl Pts',(-0.0990418820963334,-0.180786274539629,
-0.54994765810045));
#33011=CARTESIAN_POINT('Ctrl Pts',(-0.143161176789165,-0.133459935596901,
-0.553653585779475));
#33012=CARTESIAN_POINT('Ctrl Pts',(-0.176334410746974,-0.0978753296995445,
-0.556440067448842));
#33013=CARTESIAN_POINT('Ctrl Pts',(-0.194926706870171,-0.0486978554841558,
-0.559226549118209));
#33014=CARTESIAN_POINT('Ctrl Pts',(-0.195370054518654,0.000178868712723643,
-0.562013030787577));
#33015=CARTESIAN_POINT('Ctrl Pts',(-0.195340204128639,0.000177311515467854,
-0.572186969212424));
#33016=CARTESIAN_POINT('Ctrl Pts',(-0.194915250462372,-0.0477123608327619,
-0.569457821696111));
#33017=CARTESIAN_POINT('Ctrl Pts',(-0.177153235872989,-0.0958839928397431,
-0.566728674179798));
#33018=CARTESIAN_POINT('Ctrl Pts',(-0.145204503609113,-0.131233861749203,
-0.563999526663485));
#33019=CARTESIAN_POINT('Ctrl Pts',(-0.101821106229999,-0.17923568534371,
-0.560293598984461));
#33020=CARTESIAN_POINT('Ctrl Pts',(-0.0322786699314196,-0.203595324214454,
-0.556587671305437));
#33021=CARTESIAN_POINT('Ctrl Pts',(0.031575366720999,-0.193157113652105,
-0.552881743626412));
#33022=CARTESIAN_POINT('Ctrl Pts',(0.0954294033734167,-0.182718903089756,
-0.549175815947388));
#33023=CARTESIAN_POINT('Ctrl Pts',(0.153595040379674,-0.137482843094316,
-0.545469888268365));
#33024=CARTESIAN_POINT('Ctrl Pts',(0.179434922913233,-0.0781650994824409,
-0.541763960589341));
#33025=CARTESIAN_POINT('Ctrl Pts',(0.205274805446792,-0.0188473558705653,
-0.538058032910317));
#33026=CARTESIAN_POINT('Ctrl Pts',(0.198788933507652,0.0545520713577456,
-0.534352105231292));
#33027=CARTESIAN_POINT('Ctrl Pts',(0.162947556904712,0.108419408026255,
-0.530646177552268));
#33028=CARTESIAN_POINT('Ctrl Pts',(0.127106180301771,0.162286744694765,
-0.526940249873244));
#33029=CARTESIAN_POINT('Ctrl Pts',(0.0619092990350311,0.196621990803474,
-0.52323432219422));
#33030=CARTESIAN_POINT('Ctrl Pts',(-0.00278572524228628,0.195701083473885,
-0.519528394515196));
#33031=CARTESIAN_POINT('Ctrl Pts',(-0.0674807495196046,0.194780176144295,
-0.515822466836172));
#33032=CARTESIAN_POINT('Ctrl Pts',(-0.131673916807498,0.158603115376409,
-0.512116539157147));
#33033=CARTESIAN_POINT('Ctrl Pts',(-0.165967523195273,0.103737435780939,
-0.508410611478123));
#33034=CARTESIAN_POINT('Ctrl Pts',(-0.185164798177752,0.0730240857067314,
-0.506336064056223));
#33035=CARTESIAN_POINT('Ctrl Pts',(-0.194992546219555,0.0364543446917346,
-0.504261516634324));
#33036=CARTESIAN_POINT('Ctrl Pts',(-0.195097772416105,-6.2815082009945E-5,
-0.502186969212424));
#33037=CARTESIAN_POINT('Origin',(0.,0.,-0.78));
#33038=CARTESIAN_POINT('',(-0.195542596598123,-0.000155681910894878,-0.422013030787576));
#33039=CARTESIAN_POINT('',(-0.19557059622782,-0.000146131833415082,-0.432186969212424));
#33040=CARTESIAN_POINT('',(-0.1954,-2.39295984553393E-17,-0.78));
#33041=CARTESIAN_POINT('Ctrl Pts',(-0.195542596598123,-0.000155681910894878,
-0.422013030787576));
#33042=CARTESIAN_POINT('Ctrl Pts',(-0.195068207836276,0.0543592358526127,
-0.42512801131561));
#33043=CARTESIAN_POINT('Ctrl Pts',(-0.171264515120332,0.109237316871241,
-0.428242991843644));
#33044=CARTESIAN_POINT('Ctrl Pts',(-0.130811232943367,0.145585364254193,
-0.431357972371678));
#33045=CARTESIAN_POINT('Ctrl Pts',(-0.0826835041252334,0.188829048656927,
-0.435063900050703));
#33046=CARTESIAN_POINT('Ctrl Pts',(-0.0109897284654487,0.205845080920964,
-0.438769827729727));
#33047=CARTESIAN_POINT('Ctrl Pts',(0.0514374347650197,0.188840851655517,
-0.442475755408751));
#33048=CARTESIAN_POINT('Ctrl Pts',(0.113864597995486,0.171836622390071,
-0.446181683087775));
#33049=CARTESIAN_POINT('Ctrl Pts',(0.16702514879664,0.120812131595144,-0.449887610766799));
#33050=CARTESIAN_POINT('Ctrl Pts',(0.186573846106103,0.059134396913838,
-0.453593538445823));
#33051=CARTESIAN_POINT('Ctrl Pts',(0.206122543415566,-0.00254333776746921,
-0.457299466124847));
#33052=CARTESIAN_POINT('Ctrl Pts',(0.192059387233338,-0.074874316335157,
-0.461005393803871));
#33053=CARTESIAN_POINT('Ctrl Pts',(0.150824696972863,-0.124734068049718,
-0.464711321482896));
#33054=CARTESIAN_POINT('Ctrl Pts',(0.10959000671239,-0.174593819764278,
-0.46841724916192));
#33055=CARTESIAN_POINT('Ctrl Pts',(0.0411837823736688,-0.201982344625713,
-0.472123176840944));
#33056=CARTESIAN_POINT('Ctrl Pts',(-0.0230668735848738,-0.194356878685079,
-0.475829104519968));
#33057=CARTESIAN_POINT('Ctrl Pts',(-0.0873175295434183,-0.186731412744445,
-0.479535032198992));
#33058=CARTESIAN_POINT('Ctrl Pts',(-0.147412617121784,-0.144091956001744,
-0.483240959878016));
#33059=CARTESIAN_POINT('Ctrl Pts',(-0.17583117629018,-0.0859655418967326,
-0.48694688755704));
#33060=CARTESIAN_POINT('Ctrl Pts',(-0.188780924515387,-0.059478540095068,
-0.488635601967219));
#33061=CARTESIAN_POINT('Ctrl Pts',(-0.195153244509888,-0.0297757707937514,
-0.490324316377398));
#33062=CARTESIAN_POINT('Ctrl Pts',(-0.195089308542836,-4.70021948510008E-5,
-0.492013030787576));
#33063=CARTESIAN_POINT('Ctrl Pts',(-0.195097772416105,-6.2815082009945E-5,
-0.502186969212424));
#33064=CARTESIAN_POINT('Ctrl Pts',(-0.195180520073629,-0.0287791379157325,
-0.500555588955299));
#33065=CARTESIAN_POINT('Ctrl Pts',(-0.189250940656692,-0.0574629449448703,
-0.498924208698175));
#33066=CARTESIAN_POINT('Ctrl Pts',(-0.177137376206997,-0.0832407609796949,
-0.497292828441051));
#33067=CARTESIAN_POINT('Ctrl Pts',(-0.149619577343291,-0.141798979721807,
-0.493586900762027));
#33068=CARTESIAN_POINT('Ctrl Pts',(-0.0901899341282235,-0.185361118782977,
-0.489880973083003));
#33069=CARTESIAN_POINT('Ctrl Pts',(-0.0260646617536622,-0.193977595988931,
-0.486175045403978));
#33070=CARTESIAN_POINT('Ctrl Pts',(0.0380606106208982,-0.202594073194885,
-0.482469117724954));
#33071=CARTESIAN_POINT('Ctrl Pts',(0.106881512154954,-0.176264888545622,
-0.47876319004593));
#33072=CARTESIAN_POINT('Ctrl Pts',(0.148881036107087,-0.127047673830174,
-0.475057262366906));
#33073=CARTESIAN_POINT('Ctrl Pts',(0.19088056005922,-0.0778304591147251,
-0.471351334687882));
#33074=CARTESIAN_POINT('Ctrl Pts',(0.206058706429431,-0.00572521433309026,
-0.467645407008858));
#33075=CARTESIAN_POINT('Ctrl Pts',(0.187464538353933,0.0562469661201786,
-0.463939479329834));
#33076=CARTESIAN_POINT('Ctrl Pts',(0.168870370278435,0.118219146573448,
-0.46023355165081));
#33077=CARTESIAN_POINT('Ctrl Pts',(0.116503887757229,0.170058262698351,
-0.456527623971785));
#33078=CARTESIAN_POINT('Ctrl Pts',(0.0543466828045978,0.188024233560768,
-0.452821696292761));
#33079=CARTESIAN_POINT('Ctrl Pts',(-0.00781052214803026,0.205990204423184,
-0.449115768613737));
#33080=CARTESIAN_POINT('Ctrl Pts',(-0.0797584495320804,0.190083030023117,
-0.445409840934713));
#33081=CARTESIAN_POINT('Ctrl Pts',(-0.12854804954076,0.147587510641126,
-0.441703913255689));
#33082=CARTESIAN_POINT('Ctrl Pts',(-0.170312481498787,0.111210880633205,
-0.4385315985746));
#33083=CARTESIAN_POINT('Ctrl Pts',(-0.195107539066149,0.0553515145401952,
-0.435359283893512));
#33084=CARTESIAN_POINT('Ctrl Pts',(-0.19557059622782,-0.000146131833415082,
-0.432186969212424));
#33085=CARTESIAN_POINT('Origin',(0.,0.,-0.78));
#33086=CARTESIAN_POINT('',(-0.195583232845723,0.00014114408237359,-0.352013030787576));
#33087=CARTESIAN_POINT('',(-0.195555830895482,0.000151412478162425,-0.362186969212424));
#33088=CARTESIAN_POINT('',(-0.1954,-2.39295984553393E-17,-0.78));
#33089=CARTESIAN_POINT('Ctrl Pts',(-0.195583232845723,0.00014114408237359,
-0.352013030787576));
#33090=CARTESIAN_POINT('Ctrl Pts',(-0.195655424697362,0.00900615037703061,
-0.352519850895775));
#33091=CARTESIAN_POINT('Ctrl Pts',(-0.195104888905283,0.0178621385962115,
-0.353026671003973));
#33092=CARTESIAN_POINT('Ctrl Pts',(-0.193901018627014,0.0266284044659732,
-0.353533491112172));
#33093=CARTESIAN_POINT('Ctrl Pts',(-0.1850981788935,0.0907283618333217,
-0.357239418791196));
#33094=CARTESIAN_POINT('Ctrl Pts',(-0.141363472953698,0.150031130055026,
-0.36094534647022));
#33095=CARTESIAN_POINT('Ctrl Pts',(-0.0827255111732556,0.177378597216332,
-0.364651274149244));
#33096=CARTESIAN_POINT('Ctrl Pts',(-0.0240875493928135,0.204726064377639,
-0.368357201828268));
#33097=CARTESIAN_POINT('Ctrl Pts',(0.0494536682282692,0.200118230478549,
-0.372063129507292));
#33098=CARTESIAN_POINT('Ctrl Pts',(0.104219433624227,0.165665284849347,
-0.375769057186316));
#33099=CARTESIAN_POINT('Ctrl Pts',(0.158985199020186,0.131212339220144,
-0.37947498486534));
#33100=CARTESIAN_POINT('Ctrl Pts',(0.194975512191018,0.0669142818608283,
-0.383180912544365));
#33101=CARTESIAN_POINT('Ctrl Pts',(0.195708360877096,0.00221685181364163,
-0.386886840223389));
#33102=CARTESIAN_POINT('Ctrl Pts',(0.196441209563174,-0.062480578233545,
-0.390592767902413));
#33103=CARTESIAN_POINT('Ctrl Pts',(0.161916593764496,-0.127577380968602,
-0.394298695581437));
#33104=CARTESIAN_POINT('Ctrl Pts',(0.107945299515574,-0.163262026392235,
-0.398004623260461));
#33105=CARTESIAN_POINT('Ctrl Pts',(0.0539740052666519,-0.198946671815868,
-0.401710550939485));
#33106=CARTESIAN_POINT('Ctrl Pts',(-0.0194439674325147,-0.205219159928075,
-0.40541647861851));
#33107=CARTESIAN_POINT('Ctrl Pts',(-0.0786863513792303,-0.17920696151603,
-0.409122406297534));
#33108=CARTESIAN_POINT('Ctrl Pts',(-0.137928735325944,-0.153194763103985,
-0.412828333976558));
#33109=CARTESIAN_POINT('Ctrl Pts',(-0.182995530520208,-0.0948978781676894,
-0.416534261655582));
#33110=CARTESIAN_POINT('Ctrl Pts',(-0.193248087129097,-0.031013767428828,
-0.420240189334606));
#33111=CARTESIAN_POINT('Ctrl Pts',(-0.194882959593738,-0.0208268084527132,
-0.420831136485596));
#33112=CARTESIAN_POINT('Ctrl Pts',(-0.195632593529003,-0.0104977803763184,
-0.421422083636586));
#33113=CARTESIAN_POINT('Ctrl Pts',(-0.195542596598123,-0.000155681910894878,
-0.422013030787576));
#33114=CARTESIAN_POINT('Ctrl Pts',(-0.19557059622782,-0.000146131833415082,
-0.432186969212424));
#33115=CARTESIAN_POINT('Ctrl Pts',(-0.195648486773083,-0.00948135498650791,
-0.431653356214488));
#33116=CARTESIAN_POINT('Ctrl Pts',(-0.195037918301464,-0.0188063435021582,
-0.431119743216553));
#33117=CARTESIAN_POINT('Ctrl Pts',(-0.193703849275159,-0.0280266500667519,
-0.430586130218617));
#33118=CARTESIAN_POINT('Ctrl Pts',(-0.184438776367567,-0.0920614270287232,
-0.426880202539593));
#33119=CARTESIAN_POINT('Ctrl Pts',(-0.140277357919073,-0.151047116588746,
-0.423174274860568));
#33120=CARTESIAN_POINT('Ctrl Pts',(-0.0814436202345694,-0.177970815194695,
-0.419468347181544));
#33121=CARTESIAN_POINT('Ctrl Pts',(-0.0226098825500687,-0.204894513800643,
-0.41576241950252));
#33122=CARTESIAN_POINT('Ctrl Pts',(0.0508961743704401,-0.199756221452522,
-0.412056491823496));
#33123=CARTESIAN_POINT('Ctrl Pts',(0.105411944547391,-0.164909054586819,
-0.408350564144472));
#33124=CARTESIAN_POINT('Ctrl Pts',(0.159927714724343,-0.130061887721115,
-0.404644636465448));
#33125=CARTESIAN_POINT('Ctrl Pts',(0.195453198157735,-0.0655058463378307,
-0.400938708786423));
#33126=CARTESIAN_POINT('Ctrl Pts',(0.195719254573281,-0.000804815043615771,
-0.397232781107399));
#33127=CARTESIAN_POINT('Ctrl Pts',(0.195985310988826,0.0638962162505983,
-0.393526853428375));
#33128=CARTESIAN_POINT('Ctrl Pts',(0.160991940386524,0.128742237455741,
-0.389820925749351));
#33129=CARTESIAN_POINT('Ctrl Pts',(0.106764598297912,0.164036565704904,
-0.386114998070327));
#33130=CARTESIAN_POINT('Ctrl Pts',(0.052537256209301,0.199330893954067,
-0.382409070391303));
#33131=CARTESIAN_POINT('Ctrl Pts',(-0.0209240573656208,0.205073529247252,
-0.378703142712278));
#33132=CARTESIAN_POINT('Ctrl Pts',(-0.0799772269710618,0.178634592125981,
-0.374997215033254));
#33133=CARTESIAN_POINT('Ctrl Pts',(-0.139030396576502,0.152195655004712,
-0.37129128735423));
#33134=CARTESIAN_POINT('Ctrl Pts',(-0.183675422212462,0.0935751454689875,
-0.367585359675206));
#33135=CARTESIAN_POINT('Ctrl Pts',(-0.193466806325688,0.0296187303592283,
-0.363879431996182));
#33136=CARTESIAN_POINT('Ctrl Pts',(-0.194957351082485,0.0198826299159174,
-0.36331527773493));
#33137=CARTESIAN_POINT('Ctrl Pts',(-0.19564019594481,0.0100228749509908,
-0.362751123473677));
#33138=CARTESIAN_POINT('Ctrl Pts',(-0.195555830895482,0.000151412478162425,
-0.362186969212424));
#33139=CARTESIAN_POINT('Origin',(0.,0.,-0.78));
#33140=CARTESIAN_POINT('',(-0.195102573297888,7.00326263145673E-5,-0.282013030787576));
#33141=CARTESIAN_POINT('',(-0.195092954415088,5.44486870368686E-5,-0.292186969212424));
#33142=CARTESIAN_POINT('',(-0.1954,-2.39295984553393E-17,-0.78));
#33143=CARTESIAN_POINT('Ctrl Pts',(-0.195102573297888,7.00326263145673E-5,
-0.282013030787576));
#33144=CARTESIAN_POINT('Ctrl Pts',(-0.195193440705579,0.0283130019996957,
-0.283617618154963));
#33145=CARTESIAN_POINT('Ctrl Pts',(-0.189464713165188,0.0565208456325242,
-0.28522220552235));
#33146=CARTESIAN_POINT('Ctrl Pts',(-0.177733329944698,0.081960602518178,
-0.286826792889737));
#33147=CARTESIAN_POINT('Ctrl Pts',(-0.150638726887431,0.140715832121982,
-0.290532720568761));
#33148=CARTESIAN_POINT('Ctrl Pts',(-0.0915249166295698,0.184705606595511,
-0.294238648247786));
#33149=CARTESIAN_POINT('Ctrl Pts',(-0.0274634764115514,0.193784505101985,
-0.29794457592681));
#33150=CARTESIAN_POINT('Ctrl Pts',(0.0365979638064669,0.202863403608459,
-0.301650503605834));
#33151=CARTESIAN_POINT('Ctrl Pts',(0.105607033984642,0.177031426147878,
-0.305356431284858));
#33152=CARTESIAN_POINT('Ctrl Pts',(0.147960554216137,0.128118505085543,
-0.309062358963882));
#33153=CARTESIAN_POINT('Ctrl Pts',(0.190314074447633,0.0792055840232077,
-0.312768286642906));
#33154=CARTESIAN_POINT('Ctrl Pts',(0.206012044732447,0.00721171935911754,
-0.31647421432193));
#33155=CARTESIAN_POINT('Ctrl Pts',(0.187865471277307,-0.0548930018261547,
-0.320180142000955));
#33156=CARTESIAN_POINT('Ctrl Pts',(0.169718897822168,-0.116997723011427,
-0.323886069679979));
#33157=CARTESIAN_POINT('Ctrl Pts',(0.117727780627074,-0.169213300717881,
-0.327591997359002));
#33158=CARTESIAN_POINT('Ctrl Pts',(0.0557018105550347,-0.187627250821613,
-0.331297925038027));
#33159=CARTESIAN_POINT('Ctrl Pts',(-0.00632415951700459,-0.206041200925345,
-0.335003852717051));
#33160=CARTESIAN_POINT('Ctrl Pts',(-0.0783849824659894,-0.190653523426354,
-0.338709780396075));
#33161=CARTESIAN_POINT('Ctrl Pts',(-0.12747990717687,-0.148511111420363,
-0.342415708075099));
#33162=CARTESIAN_POINT('Ctrl Pts',(-0.169860643914036,-0.112132066555481,
-0.345614815645925));
#33163=CARTESIAN_POINT('Ctrl Pts',(-0.19512754946735,-0.0558158084810627,
-0.348813923216751));
#33164=CARTESIAN_POINT('Ctrl Pts',(-0.195583232845723,0.00014114408237359,
-0.352013030787576));
#33165=CARTESIAN_POINT('Ctrl Pts',(-0.195555830895482,0.000151412478162425,
-0.362186969212424));
#33166=CARTESIAN_POINT('Ctrl Pts',(-0.195086002184484,-0.0548227329316184,
-0.359045195794653));
#33167=CARTESIAN_POINT('Ctrl Pts',(-0.1708221338281,-0.110159971808954,
-0.355903422376881));
#33168=CARTESIAN_POINT('Ctrl Pts',(-0.129757467814254,-0.146525335298689,
-0.35276164895911));
#33169=CARTESIAN_POINT('Ctrl Pts',(-0.0813190025991063,-0.189420665163049,
-0.349055721280085));
#33170=CARTESIAN_POINT('Ctrl Pts',(-0.00950432957832131,-0.205919004207974,
-0.345349793601062));
#33171=CARTESIAN_POINT('Ctrl Pts',(0.052798526195835,-0.188464824223644,
-0.341643865922038));
#33172=CARTESIAN_POINT('Ctrl Pts',(0.115101381969993,-0.171010644239313,
-0.337937938243013));
#33173=CARTESIAN_POINT('Ctrl Pts',(0.167892420497522,-0.119603945225725,
-0.334232010563989));
#33174=CARTESIAN_POINT('Ctrl Pts',(0.186995621412669,-0.0577867797188634,
-0.330526082884965));
#33175=CARTESIAN_POINT('Ctrl Pts',(0.206098822327817,0.00403038578799705,
-0.326820155205941));
#33176=CARTESIAN_POINT('Ctrl Pts',(0.191514185630584,0.0762580177881299,
-0.323114227526917));
#33177=CARTESIAN_POINT('Ctrl Pts',(0.14992084633237,0.125818973819177,-0.319408299847893));
#33178=CARTESIAN_POINT('Ctrl Pts',(0.108327507034157,0.175379929850223,
-0.315702372168869));
#33179=CARTESIAN_POINT('Ctrl Pts',(0.0397254651349634,0.202274209912184,
-0.311996444489844));
#33180=CARTESIAN_POINT('Ctrl Pts',(-0.0244685008994722,0.194185392865971,
-0.30829051681082));
#33181=CARTESIAN_POINT('Ctrl Pts',(-0.0886624669339077,0.186096575819758,
-0.304584589131796));
#33182=CARTESIAN_POINT('Ctrl Pts',(-0.148448357103585,0.143024661665371,
-0.300878661452772));
#33183=CARTESIAN_POINT('Ctrl Pts',(-0.176446810473754,0.0846947307106876,
-0.297172733773748));
#33184=CARTESIAN_POINT('Ctrl Pts',(-0.189002703687302,0.0585367006746086,
-0.295510812253306));
#33185=CARTESIAN_POINT('Ctrl Pts',(-0.195165921495514,0.0293101769644822,
-0.293848890732865));
#33186=CARTESIAN_POINT('Ctrl Pts',(-0.195092954415088,5.44486870368687E-5,
-0.292186969212424));
#33187=CARTESIAN_POINT('Origin',(0.,0.,-0.78));
#33188=CARTESIAN_POINT('',(-0.195326501059731,-0.000176025207787534,-0.212013030787576));
#33189=CARTESIAN_POINT('',(-0.195356026374599,-0.000178344182095036,-0.222186969212423));
#33190=CARTESIAN_POINT('',(-0.1954,-2.39295984553393E-17,-0.78));
#33191=CARTESIAN_POINT('Ctrl Pts',(-0.195326501059731,-0.000176025207787534,
-0.212013030787576));
#33192=CARTESIAN_POINT('Ctrl Pts',(-0.194911123079697,0.04725196296477,
-0.214715385414152));
#33193=CARTESIAN_POINT('Ctrl Pts',(-0.177529267435098,0.0949526855082682,
-0.217417740040727));
#33194=CARTESIAN_POINT('Ctrl Pts',(-0.146147542718918,0.130182841238995,
-0.220120094667303));
#33195=CARTESIAN_POINT('Ctrl Pts',(-0.10311159136838,0.178496414881354,
-0.223826022346327));
#33196=CARTESIAN_POINT('Ctrl Pts',(-0.033746712246184,0.203357151128855,
-0.227531950025351));
#33197=CARTESIAN_POINT('Ctrl Pts',(0.0301809729126184,0.193379900723762,
-0.231237877704375));
#33198=CARTESIAN_POINT('Ctrl Pts',(0.0941086580714263,0.183402650318669,
-0.2349438053834));
#33199=CARTESIAN_POINT('Ctrl Pts',(0.152599149266839,0.138587413260975,
-0.238649733062424));
#33200=CARTESIAN_POINT('Ctrl Pts',(0.178866320722857,0.0794576384627894,
-0.242355660741448));
#33201=CARTESIAN_POINT('Ctrl Pts',(0.205133492178873,0.0203278636646087,
-0.246061588420472));
#33202=CARTESIAN_POINT('Ctrl Pts',(0.199177343895502,-0.0531164488740613,
-0.249767516099496));
#33203=CARTESIAN_POINT('Ctrl Pts',(0.163725535988198,-0.10724097041851,
-0.25347344377852));
#33204=CARTESIAN_POINT('Ctrl Pts',(0.128273728080893,-0.161365491962961,
-0.257179371457544));
#33205=CARTESIAN_POINT('Ctrl Pts',(0.0633262605496548,-0.196170222513189,
-0.260885299136568));
#33206=CARTESIAN_POINT('Ctrl Pts',(-0.00137372617158459,-0.195716095036698,
-0.264591226815592));
#33207=CARTESIAN_POINT('Ctrl Pts',(-0.066073712892824,-0.195261967560207,
-0.268297154494617));
#33208=CARTESIAN_POINT('Ctrl Pts',(-0.130526218804065,-0.159548982056996,
-0.272003082173641));
#33209=CARTESIAN_POINT('Ctrl Pts',(-0.16521477383135,-0.104932146938352,
-0.275709009852665));
#33210=CARTESIAN_POINT('Ctrl Pts',(-0.184883926967784,-0.073963232466964,
-0.277810350164302));
#33211=CARTESIAN_POINT('Ctrl Pts',(-0.194983574887034,-0.0369164794644935,
-0.279911690475939));
#33212=CARTESIAN_POINT('Ctrl Pts',(-0.195102573297888,7.00326263145673E-5,
-0.282013030787576));
#33213=CARTESIAN_POINT('Ctrl Pts',(-0.195092954415088,5.44486870368687E-5,
-0.292186969212424));
#33214=CARTESIAN_POINT('Ctrl Pts',(-0.195003211812967,-0.0359273278513876,
-0.290142963053841));
#33215=CARTESIAN_POINT('Ctrl Pts',(-0.185480197162667,-0.0719532811795465,
-0.288098956895258));
#33216=CARTESIAN_POINT('Ctrl Pts',(-0.16681505127669,-0.102369004125496,
-0.286054950736675));
#33217=CARTESIAN_POINT('Ctrl Pts',(-0.132973822138797,-0.157514860252015,
-0.282349023057651));
#33218=CARTESIAN_POINT('Ctrl Pts',(-0.0690803472923488,-0.194218624750074,
-0.278643095378627));
#33219=CARTESIAN_POINT('Ctrl Pts',(-0.00439508445617105,-0.195671555356572,
-0.274937167699603));
#33220=CARTESIAN_POINT('Ctrl Pts',(0.0602901783800058,-0.19712448596307,
-0.271231240020579));
#33221=CARTESIAN_POINT('Ctrl Pts',(0.125767229205913,-0.163326582678009,
-0.267525312341555));
#33222=CARTESIAN_POINT('Ctrl Pts',(0.162050400841887,-0.109755828611132,
-0.263819384662531));
#33223=CARTESIAN_POINT('Ctrl Pts',(0.198333572477861,-0.0561850745442543,
-0.260113456983507));
#33224=CARTESIAN_POINT('Ctrl Pts',(0.205422864923902,0.0171585303044398,
-0.256407529304482));
#33225=CARTESIAN_POINT('Ctrl Pts',(0.18007168767881,0.0766867761647091,
-0.252701601625458));
#33226=CARTESIAN_POINT('Ctrl Pts',(0.154720510433717,0.136215022024978,
-0.248995673946434));
#33227=CARTESIAN_POINT('Ctrl Pts',(0.0969288634974908,0.181927908896823,
-0.24528974626741));
#33228=CARTESIAN_POINT('Ctrl Pts',(0.0331628305678363,0.19289090449688,
-0.241583818588386));
#33229=CARTESIAN_POINT('Ctrl Pts',(-0.0306032023618182,0.203853900096938,
-0.237877890909362));
#33230=CARTESIAN_POINT('Ctrl Pts',(-0.100343621284901,0.180067004425208,
-0.234171963230337));
#33231=CARTESIAN_POINT('Ctrl Pts',(-0.144120320515705,0.132423591077881,
-0.230466035551313));
#33232=CARTESIAN_POINT('Ctrl Pts',(-0.176719463332301,0.0969450268354948,
-0.227706346771683));
#33233=CARTESIAN_POINT('Ctrl Pts',(-0.194920901915774,0.0482372685640377,
-0.224946657992053));
#33234=CARTESIAN_POINT('Ctrl Pts',(-0.195356026374599,-0.000178344182095036,
-0.222186969212423));
#33235=CARTESIAN_POINT('Origin',(0.,0.,-0.78));
#33236=CARTESIAN_POINT('',(-0.195715103822041,3.06823192254271E-5,-0.142013030787576));
#33237=CARTESIAN_POINT('',(-0.195706082681088,4.87745040611329E-5,-0.152186969212423));
#33238=CARTESIAN_POINT('',(-0.1954,-2.39295984553393E-17,-0.78));
#33239=CARTESIAN_POINT('Ctrl Pts',(-0.195715103822041,3.06823192254271E-5,
-0.142013030787576));
#33240=CARTESIAN_POINT('Ctrl Pts',(-0.195718688241172,0.00167534937911104,
-0.142107224994316));
#33241=CARTESIAN_POINT('Ctrl Pts',(-0.195699753624677,0.00331993167571746,
-0.142201419201056));
#33242=CARTESIAN_POINT('Ctrl Pts',(-0.19565804723958,0.00496393608527703,
-0.142295613407796));
#33243=CARTESIAN_POINT('Ctrl Pts',(-0.194017173004602,0.0696447870281606,
-0.14600154108682));
#33244=CARTESIAN_POINT('Ctrl Pts',(-0.157127667667993,0.133431121269766,
-0.149707468765844));
#33245=CARTESIAN_POINT('Ctrl Pts',(-0.101883633031363,0.167111867856658,
-0.153413396444869));
#33246=CARTESIAN_POINT('Ctrl Pts',(-0.0466395983947323,0.200792614443549,
-0.157119324123893));
#33247=CARTESIAN_POINT('Ctrl Pts',(0.0269589655419205,0.204367773375727,
-0.160825251802917));
#33248=CARTESIAN_POINT('Ctrl Pts',(0.0852072452906279,0.176199907320885,
-0.164531179481941));
#33249=CARTESIAN_POINT('Ctrl Pts',(0.143455525039335,0.148032041266044,
-0.168237107160965));
#33250=CARTESIAN_POINT('Ctrl Pts',(0.186353520600098,0.0881211502241835,
-0.171943034839989));
#33251=CARTESIAN_POINT('Ctrl Pts',(0.194255716558216,0.023903928747813,
-0.175648962519013));
#33252=CARTESIAN_POINT('Ctrl Pts',(0.202157912516335,-0.0403132927285585,
-0.179354890198038));
#33253=CARTESIAN_POINT('Ctrl Pts',(0.17506430887181,-0.108836844639439,
-0.183060817877062));
#33254=CARTESIAN_POINT('Ctrl Pts',(0.125382651628076,-0.150285940104107,
-0.186766745556086));
#33255=CARTESIAN_POINT('Ctrl Pts',(0.0757009943843419,-0.191735035568774,
-0.19047267323511));
#33256=CARTESIAN_POINT('Ctrl Pts',(0.00343128354139923,-0.206109674587227,
-0.194178600914134));
#33257=CARTESIAN_POINT('Ctrl Pts',(-0.0583300908676832,-0.186826867575142,
-0.197884528593158));
#33258=CARTESIAN_POINT('Ctrl Pts',(-0.120091465276766,-0.167544060563056,
-0.201590456272182));
#33259=CARTESIAN_POINT('Ctrl Pts',(-0.171344503251989,-0.11460380752043,
-0.205296383951207));
#33260=CARTESIAN_POINT('Ctrl Pts',(-0.188617510450161,-0.0522504754805079,
-0.209002311630231));
#33261=CARTESIAN_POINT('Ctrl Pts',(-0.193295077326858,-0.0353650613047726,
-0.210005884682679));
#33262=CARTESIAN_POINT('Ctrl Pts',(-0.195480759920963,-0.0177893504145328,
-0.211009457735128));
#33263=CARTESIAN_POINT('Ctrl Pts',(-0.195326501059731,-0.000176025207787534,
-0.212013030787576));
#33264=CARTESIAN_POINT('Ctrl Pts',(-0.195356026374599,-0.000178344182095036,
-0.222186969212423));
#33265=CARTESIAN_POINT('Ctrl Pts',(-0.195505221346168,-0.0167790335266869,
-0.221240730313029));
#33266=CARTESIAN_POINT('Ctrl Pts',(-0.193565703574764,-0.0333453765191166,
-0.220294491413635));
#33267=CARTESIAN_POINT('Ctrl Pts',(-0.189401681496759,-0.0493323163259868,
-0.219348252514241));
#33268=CARTESIAN_POINT('Ctrl Pts',(-0.173093363708484,-0.111944879359601,
-0.215642324835217));
#33269=CARTESIAN_POINT('Ctrl Pts',(-0.122663748593409,-0.165670074403903,
-0.211936397156193));
#33270=CARTESIAN_POINT('Ctrl Pts',(-0.0612074277809205,-0.185904075543387,
-0.208230469477169));
#33271=CARTESIAN_POINT('Ctrl Pts',(0.000248893031568463,-0.20613807668287,
-0.204524541798144));
#33272=CARTESIAN_POINT('Ctrl Pts',(0.0727319195414718,-0.192880883917535,
-0.20081861411912));
#33273=CARTESIAN_POINT('Ctrl Pts',(0.123047552285821,-0.15220372419822,
-0.197112686440096));
#33274=CARTESIAN_POINT('Ctrl Pts',(0.173363185030169,-0.111526564478907,
-0.193406758761072));
#33275=CARTESIAN_POINT('Ctrl Pts',(0.201511424008965,-0.0434294378056156,
-0.189700831082048));
#33276=CARTESIAN_POINT('Ctrl Pts',(0.194601583849065,0.020902114471021,
-0.185994903403024));
#33277=CARTESIAN_POINT('Ctrl Pts',(0.187691743689166,0.0852336667476595,
-0.182288975724));
#33278=CARTESIAN_POINT('Ctrl Pts',(0.145723824390569,0.145799644627643,
-0.178583048044976));
#33279=CARTESIAN_POINT('Ctrl Pts',(0.0879173338961301,0.174863425966255,
-0.174877120365952));
#33280=CARTESIAN_POINT('Ctrl Pts',(0.0301108434016909,0.203927207304867,
-0.171171192686928));
#33281=CARTESIAN_POINT('Ctrl Pts',(-0.0435342182885909,0.201488792102106,
-0.167465265007903));
#33282=CARTESIAN_POINT('Ctrl Pts',(-0.0992916054796352,0.168664897310039,
-0.163759337328879));
#33283=CARTESIAN_POINT('Ctrl Pts',(-0.155048992670679,0.135841002517972,
-0.160053409649855));
#33284=CARTESIAN_POINT('Ctrl Pts',(-0.192918705362486,0.0726316281365982,
-0.156347481970831));
#33285=CARTESIAN_POINT('Ctrl Pts',(-0.195558012150656,0.00798389026030548,
-0.152641554291807));
#33286=CARTESIAN_POINT('Ctrl Pts',(-0.195665928403547,0.00534056677067936,
-0.152490025932012));
#33287=CARTESIAN_POINT('Ctrl Pts',(-0.195714945155934,0.00269483857156378,
-0.152338497572218));
#33288=CARTESIAN_POINT('Ctrl Pts',(-0.195706082681088,4.87745040611329E-5,
-0.152186969212423));
#33289=CARTESIAN_POINT('Origin',(0.,0.,-0.78));
#33290=CARTESIAN_POINT('',(-0.195234571671998,0.00015548015543182,-0.0720130307875768));
#33291=CARTESIAN_POINT('',(-0.195211655640432,0.00014838930625368,-0.0821869692124233));
#33292=CARTESIAN_POINT('',(-0.1954,-2.39295984553393E-17,-0.78));
#33293=CARTESIAN_POINT('Ctrl Pts',(-0.195234571671998,0.00015548015543182,
-0.0720130307875768));
#33294=CARTESIAN_POINT('Ctrl Pts',(-0.195395484933967,0.0211022265122616,
-0.0732049922535051));
#33295=CARTESIAN_POINT('Ctrl Pts',(-0.192293783362919,0.0420031688312999,
-0.0743969537194334));
#33296=CARTESIAN_POINT('Ctrl Pts',(-0.185729534825066,0.0617520264313488,
-0.0755889151853617));
#33297=CARTESIAN_POINT('Ctrl Pts',(-0.165320628124816,0.123153204322723,
-0.0792948428643858));
#33298=CARTESIAN_POINT('Ctrl Pts',(-0.11144099628659,0.173417750325887,
-0.08300077054341));
#33299=CARTESIAN_POINT('Ctrl Pts',(-0.0487793746833237,0.189541935775739,
-0.0867066982224341));
#33300=CARTESIAN_POINT('Ctrl Pts',(0.013882246919943,0.205666121225591,
-0.0904126259014582));
#33301=CARTESIAN_POINT('Ctrl Pts',(0.0853258582882511,0.18764994612213,
-0.0941185535804823));
#33302=CARTESIAN_POINT('Ctrl Pts',(0.132840815824477,0.143736024314436,
-0.0978244812595064));
#33303=CARTESIAN_POINT('Ctrl Pts',(0.180355773360702,0.0998221025067421,
-0.10153040893853));
#33304=CARTESIAN_POINT('Ctrl Pts',(0.203942077064845,0.0300104339948153,
-0.105236336617555));
#33305=CARTESIAN_POINT('Ctrl Pts',(0.192794301808586,-0.0337240337379463,
-0.108942264296579));
#33306=CARTESIAN_POINT('Ctrl Pts',(0.181646526552325,-0.0974585014707116,
-0.112648191975603));
#33307=CARTESIAN_POINT('Ctrl Pts',(0.135764672335656,-0.155115768424311,
-0.116354119654627));
#33308=CARTESIAN_POINT('Ctrl Pts',(0.0761627075839468,-0.180293504362447,
-0.120060047333651));
#33309=CARTESIAN_POINT('Ctrl Pts',(0.0165607428322397,-0.205471240300582,
-0.123765975012675));
#33310=CARTESIAN_POINT('Ctrl Pts',(-0.0567613324545061,-0.198169445223256,
-0.1274719026917));
#33311=CARTESIAN_POINT('Ctrl Pts',(-0.110226248531205,-0.161730863862512,
-0.131177830370724));
#33312=CARTESIAN_POINT('Ctrl Pts',(-0.162332237560633,-0.126218448245754,
-0.134789563843008));
#33313=CARTESIAN_POINT('Ctrl Pts',(-0.195577664726791,-0.0630315725321448,
-0.138401297315292));
#33314=CARTESIAN_POINT('Ctrl Pts',(-0.195715103822041,3.06823192254271E-5,
-0.142013030787576));
#33315=CARTESIAN_POINT('Ctrl Pts',(-0.195706082681088,4.87745040611329E-5,
-0.152186969212423));
#33316=CARTESIAN_POINT('Ctrl Pts',(-0.195498195691465,-0.0620199255922364,
-0.148632569893194));
#33317=CARTESIAN_POINT('Ctrl Pts',(-0.163443397744359,-0.124273430689011,
-0.145078170573964));
#33318=CARTESIAN_POINT('Ctrl Pts',(-0.112710100455115,-0.160009726727084,
-0.141523771254734));
#33319=CARTESIAN_POINT('Ctrl Pts',(-0.0598139810868729,-0.197269504466969,
-0.13781784357571));
#33320=CARTESIAN_POINT('Ctrl Pts',(0.0133871585341446,-0.205702958575528,
-0.134111915896686));
#33321=CARTESIAN_POINT('Ctrl Pts',(0.0733704787706765,-0.181448122744779,
-0.130405988217662));
#33322=CARTESIAN_POINT('Ctrl Pts',(0.133353799007208,-0.157193286914031,
-0.126700060538638));
#33323=CARTESIAN_POINT('Ctrl Pts',(0.180119299859255,-0.100250161143975,
-0.122994132859614));
#33324=CARTESIAN_POINT('Ctrl Pts',(0.192250155136095,-0.0366958770406265,
-0.11928820518059));
#33325=CARTESIAN_POINT('Ctrl Pts',(0.204381010412935,0.026858407062722,
-0.115582277501566));
#33326=CARTESIAN_POINT('Ctrl Pts',(0.181877220114569,0.0970238494993633,
-0.111876349822541));
#33327=CARTESIAN_POINT('Ctrl Pts',(0.135045011563638,0.141667005659141,
-0.108170422143517));
#33328=CARTESIAN_POINT('Ctrl Pts',(0.0882128030127068,0.186310161818919,
-0.104464494464493));
#33329=CARTESIAN_POINT('Ctrl Pts',(0.0170521762092105,0.205431031701833,
-0.100758566785469));
#33330=CARTESIAN_POINT('Ctrl Pts',(-0.0458492466208386,0.190274405722975,
-0.0970526391064448));
#33331=CARTESIAN_POINT('Ctrl Pts',(-0.108750669450888,0.175117779744117,
-0.0933467114274207));
#33332=CARTESIAN_POINT('Ctrl Pts',(-0.16339288830749,0.125683657903486,
-0.0896407837483966));
#33333=CARTESIAN_POINT('Ctrl Pts',(-0.184750451385629,0.0646082163317357,
-0.0859348560693725));
#33334=CARTESIAN_POINT('Ctrl Pts',(-0.191950243798388,0.0440192334395667,
-0.0846855604503894));
#33335=CARTESIAN_POINT('Ctrl Pts',(-0.195367521513062,0.0221073147393436,
-0.0834362648314064));
#33336=CARTESIAN_POINT('Ctrl Pts',(-0.195211655640432,0.00014838930625368,
-0.0821869692124233));
#33337=CARTESIAN_POINT('Origin',(0.,0.,-1.69400562256037));
#33338=CARTESIAN_POINT('',(-0.155418309230191,0.000123771433864409,-0.0490056225603702));
#33339=CARTESIAN_POINT('',(-0.155328830661012,-0.000161474934390352,-0.0351943774396294));
#33340=CARTESIAN_POINT('',(-0.15555,-7.70311135908521E-15,-1.69400562256037));
#33341=CARTESIAN_POINT('',(0.133820275402922,-0.0797997733406099,-0.0200000000000001));
#33342=CARTESIAN_POINT('Ctrl Pts',(-0.155418309230191,0.000123771433864406,
-0.0490056225603702));
#33343=CARTESIAN_POINT('Ctrl Pts',(-0.155148140851959,-0.0350451663106925,
-0.0464916563472745));
#33344=CARTESIAN_POINT('Ctrl Pts',(-0.125895296854632,-0.122459193602597,
-0.0402717624551546));
#33345=CARTESIAN_POINT('Ctrl Pts',(0.0153022004281231,-0.181264675260222,
-0.030603221601698));
#33346=CARTESIAN_POINT('Ctrl Pts',(0.10904323201914,-0.120867443416895,
-0.023448646961337));
#33347=CARTESIAN_POINT('Ctrl Pts',(0.133821766704343,-0.0798002879704671,
-0.0200000000000001));
#33348=CARTESIAN_POINT('',(-0.0319621170202007,-0.152230829911641,-0.02));
#33349=CARTESIAN_POINT('Origin',(0.,0.,-0.02));
#33350=CARTESIAN_POINT('Ctrl Pts',(-0.155328830661012,-0.000161474934390372,
-0.0351943774396294));
#33351=CARTESIAN_POINT('Ctrl Pts',(-0.155437122863521,-0.0191944279743207,
-0.0338355126387771));
#33352=CARTESIAN_POINT('Ctrl Pts',(-0.14338792007184,-0.089950127265619,
-0.0287707201589006));
#33353=CARTESIAN_POINT('Ctrl Pts',(-0.0826006812134621,-0.141598846131356,
-0.0237059276790242));
#33354=CARTESIAN_POINT('Ctrl Pts',(-0.0319621170202007,-0.152230829911641,
-0.02));
#33355=CARTESIAN_POINT('Origin',(0.,0.,-1.69400562256037));
#33356=CARTESIAN_POINT('',(-0.15580084134861,2.44249475701479E-5,-0.11900562256037));
#33357=CARTESIAN_POINT('',(-0.155400066708645,0.000118126696958647,-0.105194377439629));
#33358=CARTESIAN_POINT('',(-0.15555,-7.70311135908521E-15,-1.69400562256037));
#33359=CARTESIAN_POINT('Ctrl Pts',(-0.15580084134861,2.44249475701479E-5,
-0.11900562256037));
#33360=CARTESIAN_POINT('Ctrl Pts',(-0.155691431669664,-0.0501768736303758,
-0.115393889088086));
#33361=CARTESIAN_POINT('Ctrl Pts',(-0.10207054701376,-0.15208972189888,
-0.108076227936777));
#33362=CARTESIAN_POINT('Ctrl Pts',(0.0715520591525512,-0.169379967518084,
-0.0970526391064447));
#33363=CARTESIAN_POINT('Ctrl Pts',(0.181126098406431,-0.0316841454920027,
-0.0859348560693724));
#33364=CARTESIAN_POINT('Ctrl Pts',(0.124797804529567,0.135038552108262,
-0.0748170730322999));
#33365=CARTESIAN_POINT('Ctrl Pts',(-0.0458222632545728,0.17806438686788,
-0.0636992899952276));
#33366=CARTESIAN_POINT('Ctrl Pts',(-0.145400467791554,0.0851674409887763,
-0.055095473171251));
#33367=CARTESIAN_POINT('Ctrl Pts',(-0.155546405739399,0.0167986250459671,
-0.0501975840262985));
#33368=CARTESIAN_POINT('Ctrl Pts',(-0.155418309230191,0.000123771433864406,
-0.0490056225603702));
#33369=CARTESIAN_POINT('Ctrl Pts',(-0.155400066708645,0.000118126696958645,
-0.105194377439629));
#33370=CARTESIAN_POINT('Ctrl Pts',(-0.155156077066721,-0.0342559813938016,
-0.102737745379588));
#33371=CARTESIAN_POINT('Ctrl Pts',(-0.126953063311157,-0.120847780513784,
-0.0965751856405233));
#33372=CARTESIAN_POINT('Ctrl Pts',(0.016274431326597,-0.183144050045734,
-0.0867066982224341));
#33373=CARTESIAN_POINT('Ctrl Pts',(0.162746700955473,-0.0856111115207315,
-0.0755889151853617));
#33374=CARTESIAN_POINT('Ctrl Pts',(0.160120950075793,0.0903886722456795,
-0.0644711321482895));
#33375=CARTESIAN_POINT('Ctrl Pts',(0.0109069706335314,0.18349634534749,
-0.0533533491112173));
#33376=CARTESIAN_POINT('Ctrl Pts',(-0.128953969743316,0.117874527456855,
-0.0435944308749972));
#33377=CARTESIAN_POINT('Ctrl Pts',(-0.155141785851002,0.0327126840798016,
-0.0375414403178012));
#33378=CARTESIAN_POINT('Ctrl Pts',(-0.155328830661012,-0.000161474934390372,
-0.0351943774396294));
#33379=CARTESIAN_POINT('Origin',(0.,0.,-1.69400562256037));
#33380=CARTESIAN_POINT('',(-0.155491490480251,-0.00014012651520363,-0.18900562256037));
#33381=CARTESIAN_POINT('',(-0.155793659984868,3.88274007404833E-5,-0.175194377439629));
#33382=CARTESIAN_POINT('',(-0.15555,-7.70311135908521E-15,-1.69400562256037));
#33383=CARTESIAN_POINT('Ctrl Pts',(-0.155491490480251,-0.000140126515203627,
-0.18900562256037));
#33384=CARTESIAN_POINT('Ctrl Pts',(-0.155614289691432,-0.0141613790019463,
-0.188002049507921));
#33385=CARTESIAN_POINT('Ctrl Pts',(-0.147449247613328,-0.0798188625535115,
-0.183292548776449));
#33386=CARTESIAN_POINT('Ctrl Pts',(-0.0547994747530945,-0.175518602770541,
-0.174877120365952));
#33387=CARTESIAN_POINT('Ctrl Pts',(0.11779346570166,-0.141189404725702,
-0.163759337328879));
#33388=CARTESIAN_POINT('Ctrl Pts',(0.182497816472988,0.0224570410225731,
-0.152641554291807));
#33389=CARTESIAN_POINT('Ctrl Pts',(0.080049763103335,0.16553491873334,-0.141523771254734));
#33390=CARTESIAN_POINT('Ctrl Pts',(-0.0957167152029026,0.156996802481032,
-0.130405988217662));
#33391=CARTESIAN_POINT('Ctrl Pts',(-0.155195594339883,0.054150759132695,
-0.122899938652874));
#33392=CARTESIAN_POINT('Ctrl Pts',(-0.155803694759029,0.00133367756356404,
-0.11909981676711));
#33393=CARTESIAN_POINT('Ctrl Pts',(-0.15580084134861,2.44249475701479E-5,
-0.11900562256037));
#33394=CARTESIAN_POINT('Ctrl Pts',(-0.155793659984868,3.88274007404889E-5,
-0.175194377439629));
#33395=CARTESIAN_POINT('Ctrl Pts',(-0.155628169599829,-0.0493715426093849,
-0.1716399781204));
#33396=CARTESIAN_POINT('Ctrl Pts',(-0.10350528241731,-0.150599209937992,
-0.164379651122146));
#33397=CARTESIAN_POINT('Ctrl Pts',(0.0689294256808382,-0.170465296791246,
-0.153413396444868));
#33398=CARTESIAN_POINT('Ctrl Pts',(0.18061377047412,-0.0344749710973018,
-0.142295613407796));
#33399=CARTESIAN_POINT('Ctrl Pts',(0.126870711401792,0.133092601640971,
-0.131177830370724));
#33400=CARTESIAN_POINT('Ctrl Pts',(-0.0430735388430987,0.178756644275882,
-0.120060047333651));
#33401=CARTESIAN_POINT('Ctrl Pts',(-0.144734088084764,0.0867856357268612,
-0.11139889635662));
#33402=CARTESIAN_POINT('Ctrl Pts',(-0.1555241451963,0.0175987349421875,
-0.106443673058612));
#33403=CARTESIAN_POINT('Ctrl Pts',(-0.155400066708645,0.000118126696958645,
-0.105194377439629));
#33404=CARTESIAN_POINT('Origin',(0.,0.,-1.69400562256037));
#33405=CARTESIAN_POINT('',(-0.155313230688262,5.57501280555406E-5,-0.259005622560369));
#33406=CARTESIAN_POINT('',(-0.155514994383668,-0.000141972556441383,-0.245194377439629));
#33407=CARTESIAN_POINT('',(-0.15555,-7.70311135908521E-15,-1.69400562256037));
#33408=CARTESIAN_POINT('Ctrl Pts',(-0.155313230688262,5.57501280555421E-5,
-0.259005622560369));
#33409=CARTESIAN_POINT('Ctrl Pts',(-0.155218500888833,-0.02938770921547,
-0.256904282248733));
#33410=CARTESIAN_POINT('Ctrl Pts',(-0.132999364931809,-0.110890237651056,
-0.251097014258072));
#33411=CARTESIAN_POINT('Ctrl Pts',(-0.0012905770009465,-0.183869774559952,
-0.241583818588386));
#33412=CARTESIAN_POINT('Ctrl Pts',(0.153815542361654,-0.100749879415303,
-0.230466035551314));
#33413=CARTESIAN_POINT('Ctrl Pts',(0.168039885229795,0.0746482190809691,
-0.219348252514241));
#33414=CARTESIAN_POINT('Ctrl Pts',(0.0283541753201865,0.181674986598733,
-0.208230469477169));
#33415=CARTESIAN_POINT('Ctrl Pts',(-0.122348206378289,0.127662463104303,
-0.198116259492545));
#33416=CARTESIAN_POINT('Ctrl Pts',(-0.155160824949062,0.0376153676518437,
-0.191707977186946));
#33417=CARTESIAN_POINT('Ctrl Pts',(-0.155491490480251,-0.000140126515203627,
-0.18900562256037));
#33418=CARTESIAN_POINT('Ctrl Pts',(-0.155514994383668,-0.000141972556441401,
-0.245194377439629));
#33419=CARTESIAN_POINT('Ctrl Pts',(-0.155633762438056,-0.0133571067813652,
-0.244248138540235));
#33420=CARTESIAN_POINT('Ctrl Pts',(-0.148042855299553,-0.0781946520382958,
-0.239595971961817));
#33421=CARTESIAN_POINT('Ctrl Pts',(-0.0575026584572911,-0.174651658969645,
-0.231237877704375));
#33422=CARTESIAN_POINT('Ctrl Pts',(0.115599717800877,-0.142991121590197,
-0.220120094667303));
#33423=CARTESIAN_POINT('Ctrl Pts',(0.182822725577002,0.0196369447459957,
-0.209002311630231));
#33424=CARTESIAN_POINT('Ctrl Pts',(0.0825958599644629,0.164279286494686,
-0.197884528593158));
#33425=CARTESIAN_POINT('Ctrl Pts',(-0.0932816632585158,0.158455916717979,
-0.186766745556086));
#33426=CARTESIAN_POINT('Ctrl Pts',(-0.154807377033864,0.0557616631925561,
-0.179203361838243));
#33427=CARTESIAN_POINT('Ctrl Pts',(-0.15580071504097,0.0021452514831387,
-0.175345905799424));
#33428=CARTESIAN_POINT('Ctrl Pts',(-0.155793659984868,3.88274007404889E-5,
-0.175194377439629));
#33429=CARTESIAN_POINT('Origin',(0.,0.,-1.69400562256037));
#33430=CARTESIAN_POINT('',(-0.155695864222888,0.0001123590686367,-0.32900562256037));
#33431=CARTESIAN_POINT('',(-0.155305573486524,4.33443872281669E-5,-0.315194377439629));
#33432=CARTESIAN_POINT('',(-0.15555,-7.70311135908521E-15,-1.69400562256037));
#33433=CARTESIAN_POINT('Ctrl Pts',(-0.155695864222888,0.000112359068636702,
-0.32900562256037));
#33434=CARTESIAN_POINT('Ctrl Pts',(-0.155333113201872,-0.044432697078968,
-0.325806514989544));
#33435=CARTESIAN_POINT('Ctrl Pts',(-0.111918636618463,-0.141197251894673,
-0.318901479739694));
#33436=CARTESIAN_POINT('Ctrl Pts',(0.0523302865754574,-0.176270532440662,
-0.30829051681082));
#33437=CARTESIAN_POINT('Ctrl Pts',(0.176494333858419,-0.0515704334810062,
-0.297172733773748));
#33438=CARTESIAN_POINT('Ctrl Pts',(0.139004785069224,0.12036373717149,-0.286054950736676));
#33439=CARTESIAN_POINT('Ctrl Pts',(-0.0258011647703144,0.182055099924714,
-0.274937167699603));
#33440=CARTESIAN_POINT('Ctrl Pts',(-0.140292520438531,0.0968559071634296,
-0.265920724974167));
#33441=CARTESIAN_POINT('Ctrl Pts',(-0.155385566539166,0.0225388304045638,
-0.260610209927757));
#33442=CARTESIAN_POINT('Ctrl Pts',(-0.155313230688262,5.57501280555421E-5,
-0.259005622560369));
#33443=CARTESIAN_POINT('Ctrl Pts',(-0.155305573486524,4.33443872281461E-5,
-0.315194377439629));
#33444=CARTESIAN_POINT('Ctrl Pts',(-0.155234133047627,-0.0286002858100627,
-0.313150371281046));
#33445=CARTESIAN_POINT('Ctrl Pts',(-0.133908567567703,-0.10927577092568,
-0.30740043744344));
#33446=CARTESIAN_POINT('Ctrl Pts',(-0.00412905838771584,-0.183827930642512,
-0.29794457592681));
#33447=CARTESIAN_POINT('Ctrl Pts',(0.152241800199334,-0.103112518319205,
-0.286826792889737));
#33448=CARTESIAN_POINT('Ctrl Pts',(0.169172293136615,0.0720450722777397,
-0.275709009852665));
#33449=CARTESIAN_POINT('Ctrl Pts',(0.031155547779449,0.181215587419735,
-0.264591226815592));
#33450=CARTESIAN_POINT('Ctrl Pts',(-0.12122164066584,0.129243139587191,
-0.254419682677914));
#33451=CARTESIAN_POINT('Ctrl Pts',(-0.155168609483109,0.0383997294019111,
-0.247954066219259));
#33452=CARTESIAN_POINT('Ctrl Pts',(-0.155514994383668,-0.000141972556441401,
-0.245194377439629));
#33453=CARTESIAN_POINT('Origin',(0.,0.,-1.69400562256037));
#33454=CARTESIAN_POINT('',(-0.155663515357411,-0.000123932043195673,-0.39900562256037));
#33455=CARTESIAN_POINT('',(-0.155674050643768,0.000120533321258946,-0.385194377439629));
#33456=CARTESIAN_POINT('',(-0.15555,-7.70311135908521E-15,-1.69400562256037));
#33457=CARTESIAN_POINT('Ctrl Pts',(-0.155663515357411,-0.000123932043195673,
-0.39900562256037));
#33458=CARTESIAN_POINT('Ctrl Pts',(-0.155735158257095,-0.00835685638452879,
-0.39841467540938));
#33459=CARTESIAN_POINT('Ctrl Pts',(-0.1513960673005,-0.068144160838432,
-0.394117800579365));
#33460=CARTESIAN_POINT('Ctrl Pts',(-0.0739236171314337,-0.168359907127257,
-0.386114998070327));
#33461=CARTESIAN_POINT('Ctrl Pts',(0.101411577137068,-0.153380088408926,
-0.374997215033255));
#33462=CARTESIAN_POINT('Ctrl Pts',(0.183862508367636,0.00208267001642915,
-0.363879431996182));
#33463=CARTESIAN_POINT('Ctrl Pts',(0.0979112307772101,0.155637882230987,
-0.35276164895911));
#33464=CARTESIAN_POINT('Ctrl Pts',(-0.0777182943142881,0.166642210219781,
-0.341643865922037));
#33465=CARTESIAN_POINT('Ctrl Pts',(-0.152110471914154,0.0657689570239066,
-0.333725190455791));
#33466=CARTESIAN_POINT('Ctrl Pts',(-0.155753333222491,0.00716943035386869,
-0.329512442668568));
#33467=CARTESIAN_POINT('Ctrl Pts',(-0.155695864222888,0.000112359068636702,
-0.32900562256037));
#33468=CARTESIAN_POINT('Ctrl Pts',(-0.155674050643768,0.00012053332125895,
-0.385194377439629));
#33469=CARTESIAN_POINT('Ctrl Pts',(-0.155300039098235,-0.0436421499872883,
-0.382052604021858));
#33470=CARTESIAN_POINT('Ctrl Pts',(-0.113200685144466,-0.139655777002699,
-0.375204902925063));
#33471=CARTESIAN_POINT('Ctrl Pts',(0.0496027324589358,-0.177057409124813,
-0.364651274149244));
#33472=CARTESIAN_POINT('Ctrl Pts',(0.175677134346707,-0.054289056541952,
-0.353533491112171));
#33473=CARTESIAN_POINT('Ctrl Pts',(0.140846424445151,0.118203392142091,
-0.342415708075099));
#33474=CARTESIAN_POINT('Ctrl Pts',(-0.0229874693739835,0.182431722699479,
-0.331297925038026));
#33475=CARTESIAN_POINT('Ctrl Pts',(-0.139516816184985,0.0984797733671933,
-0.322224148159537));
#33476=CARTESIAN_POINT('Ctrl Pts',(-0.155363659614267,0.0233326408742186,
-0.316856298960071));
#33477=CARTESIAN_POINT('Ctrl Pts',(-0.155305573486524,4.33443872281461E-5,
-0.315194377439629));
#33478=CARTESIAN_POINT('Origin',(0.,0.,-1.69400562256037));
#33479=CARTESIAN_POINT('',(-0.155302671155773,-3.74165374094889E-5,-0.46900562256037));
#33480=CARTESIAN_POINT('',(-0.155685804724859,-0.000116329614590766,-0.455194377439629));
#33481=CARTESIAN_POINT('',(-0.15555,-7.70311135908521E-15,-1.69400562256037));
#33482=CARTESIAN_POINT('Ctrl Pts',(-0.155302671155773,-3.74165374095008E-5,
-0.46900562256037));
#33483=CARTESIAN_POINT('Ctrl Pts',(-0.155353567981131,-0.0237032812024999,
-0.467316908150191));
#33484=CARTESIAN_POINT('Ctrl Pts',(-0.139148552154265,-0.0992383841234035,
-0.461922266060988));
#33485=CARTESIAN_POINT('Ctrl Pts',(-0.0216706798754521,-0.182592828806171,
-0.452821696292762));
#33486=CARTESIAN_POINT('Ctrl Pts',(0.141695566734905,-0.117184153644509,
-0.441703913255688));
#33487=CARTESIAN_POINT('Ctrl Pts',(0.175280888292921,0.0555551050484869,
-0.430586130218617));
#33488=CARTESIAN_POINT('Ctrl Pts',(0.0483240252869895,0.177410676335346,
-0.419468347181544));
#33489=CARTESIAN_POINT('Ctrl Pts',(-0.113792699461829,0.138933369296078,
-0.408941511295462));
#33490=CARTESIAN_POINT('Ctrl Pts',(-0.155285873740701,0.0432731787966904,
-0.402120603088404));
#33491=CARTESIAN_POINT('Ctrl Pts',(-0.155663515357411,-0.000123932043195673,
-0.39900562256037));
#33492=CARTESIAN_POINT('Ctrl Pts',(-0.155685804724859,-0.000116329614590777,
-0.455194377439629));
#33493=CARTESIAN_POINT('Ctrl Pts',(-0.155747810222891,-0.00754772143374497,
-0.454660764441694));
#33494=CARTESIAN_POINT('Ctrl Pts',(-0.15188616619471,-0.0665251955223991,
-0.450421223764734));
#33495=CARTESIAN_POINT('Ctrl Pts',(-0.0765139937801866,-0.167198582376871,
-0.44247575540875));
#33496=CARTESIAN_POINT('Ctrl Pts',(0.0990315612963532,-0.154927425139147,
-0.431357972371679));
#33497=CARTESIAN_POINT('Ctrl Pts',(0.183872742689355,-0.000756101129370498,
-0.420240189334605));
#33498=CARTESIAN_POINT('Ctrl Pts',(0.100302341504276,0.154107746339307,
-0.409122406297534));
#33499=CARTESIAN_POINT('Ctrl Pts',(-0.0751363584943781,0.167822182161027,
-0.398004623260461));
#33500=CARTESIAN_POINT('Ctrl Pts',(-0.15162681660732,0.0673874850065461,
-0.390028613641159));
#33501=CARTESIAN_POINT('Ctrl Pts',(-0.155741210231399,0.00797880347299771,
-0.385758531700882));
#33502=CARTESIAN_POINT('Ctrl Pts',(-0.155674050643768,0.00012053332125895,
-0.385194377439629));
#33503=CARTESIAN_POINT('Origin',(0.,0.,-1.69400562256037));
#33504=CARTESIAN_POINT('',(-0.155526161619123,0.000142390113939882,-0.53900562256037));
#33505=CARTESIAN_POINT('',(-0.155309408901357,-5.00045343397038E-5,-0.525194377439629));
#33506=CARTESIAN_POINT('',(-0.15555,-7.70311135908521E-15,-1.69400562256037));
#33507=CARTESIAN_POINT('Ctrl Pts',(-0.155526161619123,0.000142390113939881,
-0.53900562256037));
#33508=CARTESIAN_POINT('Ctrl Pts',(-0.155173230571418,-0.0387663839332682,
-0.536219140891002));
#33509=CARTESIAN_POINT('Ctrl Pts',(-0.120688392748538,-0.129980358346068,
-0.529726731542611));
#33510=CARTESIAN_POINT('Ctrl Pts',(0.032462156090606,-0.180986098691733,
-0.519528394515196));
#33511=CARTESIAN_POINT('Ctrl Pts',(0.169687680181897,-0.0708226707501974,
-0.508410611478123));
#33512=CARTESIAN_POINT('Ctrl Pts',(0.151493916207583,0.104208218724794,
-0.497292828441051));
#33513=CARTESIAN_POINT('Ctrl Pts',(-0.00545521632391679,0.183793362536746,
-0.486175045403978));
#33514=CARTESIAN_POINT('Ctrl Pts',(-0.13432728737953,0.108520707887271,
-0.476745976777085));
#33515=CARTESIAN_POINT('Ctrl Pts',(-0.155241873574587,0.0282320741078864,
-0.471022835829215));
#33516=CARTESIAN_POINT('Ctrl Pts',(-0.155302671155773,-3.74165374095008E-5,
-0.46900562256037));
#33517=CARTESIAN_POINT('Ctrl Pts',(-0.155309408901357,-5.00045343397228E-5,
-0.525194377439629));
#33518=CARTESIAN_POINT('Ctrl Pts',(-0.155375280949092,-0.0229099022660926,
-0.523562997182505));
#33519=CARTESIAN_POINT('Ctrl Pts',(-0.139932112659729,-0.0976148396626936,
-0.518225689246357));
#33520=CARTESIAN_POINT('Ctrl Pts',(-0.0244870176639766,-0.182236503365697,
-0.509182453631186));
#33521=CARTESIAN_POINT('Ctrl Pts',(0.139869551941277,-0.119357721295182,
-0.498064670594112));
#33522=CARTESIAN_POINT('Ctrl Pts',(0.176117668643726,0.0528424449143884,
-0.486946887557041));
#33523=CARTESIAN_POINT('Ctrl Pts',(0.0510571821108666,0.176643486570915,
-0.475829104519967));
#33524=CARTESIAN_POINT('Ctrl Pts',(-0.112520335133757,0.140477662351258,
-0.465244934480831));
#33525=CARTESIAN_POINT('Ctrl Pts',(-0.155317183734598,0.0440630915390226,
-0.458366692120718));
#33526=CARTESIAN_POINT('Ctrl Pts',(-0.155685804724859,-0.000116329614590777,
-0.455194377439629));
#33527=CARTESIAN_POINT('Origin',(0.,0.,-1.69400562256037));
#33528=CARTESIAN_POINT('',(-0.155789325782022,-4.54178512007087E-5,-0.60900562256037));
#33529=CARTESIAN_POINT('',(-0.15550239893659,0.000141150492465145,-0.595194377439629));
#33530=CARTESIAN_POINT('',(-0.15555,-7.70311135908521E-15,-1.69400562256037));
#33531=CARTESIAN_POINT('Ctrl Pts',(-0.155789325782022,-4.54178512007122E-5,
-0.60900562256037));
#33532=CARTESIAN_POINT('Ctrl Pts',(-0.155798887408862,-0.00252447849977371,
-0.608827301310838));
#33533=CARTESIAN_POINT('Ctrl Pts',(-0.154621603582211,-0.0565148725602989,
-0.604943052382282));
#33534=CARTESIAN_POINT('Ctrl Pts',(-0.0921360414391275,-0.159124823222627,
-0.597352875774703));
#33535=CARTESIAN_POINT('Ctrl Pts',(0.0837789491030789,-0.163679098191823,
-0.58623509273763));
#33536=CARTESIAN_POINT('Ctrl Pts',(0.182959643964377,-0.01831742826199,
-0.575117309700558));
#33537=CARTESIAN_POINT('Ctrl Pts',(0.114565075971008,0.143821427003983,
-0.563999526663485));
#33538=CARTESIAN_POINT('Ctrl Pts',(-0.0587612261677574,0.174232252459085,
-0.552881743626413));
#33539=CARTESIAN_POINT('Ctrl Pts',(-0.14831515963045,0.0774358242001071,
-0.544550442258708));
#33540=CARTESIAN_POINT('Ctrl Pts',(-0.155642617093086,0.012980987773357,
-0.539925068570027));
#33541=CARTESIAN_POINT('Ctrl Pts',(-0.155526161619123,0.000142390113939881,
-0.53900562256037));
#33542=CARTESIAN_POINT('Ctrl Pts',(-0.15550239893659,0.000141150492465129,
-0.595194377439629));
#33543=CARTESIAN_POINT('Ctrl Pts',(-0.155164110590692,-0.0379818716864814,
-0.592465229923317));
#33544=CARTESIAN_POINT('Ctrl Pts',(-0.121824210522794,-0.128401648628898,
-0.58603015472798));
#33545=CARTESIAN_POINT('Ctrl Pts',(0.0296641702068159,-0.181465683254363,
-0.575889151853619));
#33546=CARTESIAN_POINT('Ctrl Pts',(0.168574070457431,-0.0734339156142763,
-0.564771368816547));
#33547=CARTESIAN_POINT('Ctrl Pts',(0.153084653157532,0.101856988766946,
-0.553653585779474));
#33548=CARTESIAN_POINT('Ctrl Pts',(-0.00261711062509075,0.183855671451842,
-0.542535802742403));
#33549=CARTESIAN_POINT('Ctrl Pts',(-0.133426488682267,0.110136005965318,
-0.533049399962453));
#33550=CARTESIAN_POINT('Ctrl Pts',(-0.155225642602111,0.0290198225015199,
-0.527268924861529));
#33551=CARTESIAN_POINT('Ctrl Pts',(-0.155309408901357,-5.00045343397228E-5,
-0.525194377439629));
#33552=CARTESIAN_POINT('Origin',(0.,0.,-1.69400562256037));
#33553=CARTESIAN_POINT('',(-0.155391605265501,-0.00011484305413676,-0.67900562256037));
#33554=CARTESIAN_POINT('',(-0.15579782156367,-3.11631852267236E-5,-0.665194377439629));
#33555=CARTESIAN_POINT('',(-0.15555,-7.70311135908521E-15,-1.69400562256037));
#33556=CARTESIAN_POINT('Ctrl Pts',(-0.155391605265501,-0.000114843054136771,
-0.67900562256037));
#33557=CARTESIAN_POINT('Ctrl Pts',(-0.155513806205127,-0.0179724822621975,
-0.67772953405165));
#33558=CARTESIAN_POINT('Ctrl Pts',(-0.144419737971622,-0.0875438573516224,
-0.672747517863905));
#33559=CARTESIAN_POINT('Ctrl Pts',(-0.041783515845475,-0.179063947519582,
-0.664059573997137));
#33560=CARTESIAN_POINT('Ctrl Pts',(0.127828044966229,-0.132173183429228,
-0.652941790960064));
#33561=CARTESIAN_POINT('Ctrl Pts',(0.180360135293257,0.0357768234294574,
-0.641824007922992));
#33562=CARTESIAN_POINT('Ctrl Pts',(0.0676978886322038,0.170958343968484,
-0.630706224885919));
#33563=CARTESIAN_POINT('Ctrl Pts',(-0.104168244489674,0.149900024002337,
-0.619766763098379));
#33564=CARTESIAN_POINT('Ctrl Pts',(-0.155600174705506,0.0489961310722934,
-0.612533228989862));
#33565=CARTESIAN_POINT('Ctrl Pts',(-0.155789325782022,-4.54178512007122E-5,
-0.60900562256037));
#33566=CARTESIAN_POINT('Ctrl Pts',(-0.15579782156367,-3.11631852267405E-5,
-0.665194377439629));
#33567=CARTESIAN_POINT('Ctrl Pts',(-0.155802429055179,-0.00171290653077161,
-0.665073390343152));
#33568=CARTESIAN_POINT('Ctrl Pts',(-0.155015687096898,-0.0549033244907316,
-0.661246475567651));
#33569=CARTESIAN_POINT('Ctrl Pts',(-0.0945816730450154,-0.157683430699099,
-0.653713633113126));
#33570=CARTESIAN_POINT('Ctrl Pts',(0.081242036168499,-0.164952989521948,
-0.642595850076053));
#33571=CARTESIAN_POINT('Ctrl Pts',(0.182655043268737,-0.0211398287960793,
-0.631478067038982));
#33572=CARTESIAN_POINT('Ctrl Pts',(0.116771775495109,0.142035592865843,
-0.620360284001909));
#33573=CARTESIAN_POINT('Ctrl Pts',(-0.0560643729717556,0.175118654849549,
-0.609242500964836));
#33574=CARTESIAN_POINT('Ctrl Pts',(-0.147728502578342,0.0790597880150364,
-0.600853865444076));
#33575=CARTESIAN_POINT('Ctrl Pts',(-0.155623474599805,0.0137856352938298,
-0.596171157602341));
#33576=CARTESIAN_POINT('Ctrl Pts',(-0.15550239893659,0.000141150492465129,
-0.595194377439629));
#33577=CARTESIAN_POINT('Origin',(0.,0.,-1.69400562256037));
#33578=CARTESIAN_POINT('',(-0.155374470604174,0.000106635008702182,-0.74900562256037));
#33579=CARTESIAN_POINT('',(-0.15541051600741,-0.000122268189293742,-0.735194377439629));
#33580=CARTESIAN_POINT('',(-0.15555,-7.70311135908521E-15,-1.69400562256037));
#33581=CARTESIAN_POINT('Ctrl Pts',(-0.155374470604174,0.000106635008702186,
-0.74900562256037));
#33582=CARTESIAN_POINT('Ctrl Pts',(-0.155164878665456,-0.0331224170312113,
-0.746631766792461));
#33583=CARTESIAN_POINT('Ctrl Pts',(-0.12842734549985,-0.118534576453168,
-0.740551983345528));
#33584=CARTESIAN_POINT('Ctrl Pts',(0.0121936665653112,-0.183469545138692,
-0.730766272219571));
#33585=CARTESIAN_POINT('Ctrl Pts',(0.160788251222258,-0.0892014448683006,
-0.719648489182499));
#33586=CARTESIAN_POINT('Ctrl Pts',(0.162114657614943,0.0867674897879067,
-0.708530706145426));
#33587=CARTESIAN_POINT('Ctrl Pts',(0.014958011823137,0.183264883106403,
-0.697412923108354));
#33588=CARTESIAN_POINT('Ctrl Pts',(-0.12743588276431,0.120097779836716,
-0.687571228580002));
#33589=CARTESIAN_POINT('Ctrl Pts',(-0.155158918717726,0.0338884341013097,
-0.681435461730674));
#33590=CARTESIAN_POINT('Ctrl Pts',(-0.155391605265501,-0.000114843054136771,
-0.67900562256037));
#33591=CARTESIAN_POINT('Ctrl Pts',(-0.15541051600741,-0.000122268189293732,
-0.735194377439629));
#33592=CARTESIAN_POINT('Ctrl Pts',(-0.155535777391527,-0.0171723439086348,
-0.733975623083964));
#33593=CARTESIAN_POINT('Ctrl Pts',(-0.145086129026133,-0.085918178416682,
-0.729050941049274));
#33594=CARTESIAN_POINT('Ctrl Pts',(-0.0445429760552296,-0.17839753495263,
-0.72042033133556));
#33595=CARTESIAN_POINT('Ctrl Pts',(0.125772278341771,-0.134130873380261,
-0.709302548298488));
#33596=CARTESIAN_POINT('Ctrl Pts',(0.180890967276192,0.032988106203831,
-0.698184765261415));
#33597=CARTESIAN_POINT('Ctrl Pts',(0.0703291228835756,0.169892824061108,
-0.687066982224344));
#33598=CARTESIAN_POINT('Ctrl Pts',(-0.102743979992633,0.151393885647765,
-0.676070186283748));
#33599=CARTESIAN_POINT('Ctrl Pts',(-0.155661298051869,0.0498001836643546,
-0.668779318022176));
#33600=CARTESIAN_POINT('Ctrl Pts',(-0.15579782156367,-3.11631852267405E-5,
-0.665194377439629));
#33601=CARTESIAN_POINT('Origin',(0.,0.,-1.69400562256037));
#33602=CARTESIAN_POINT('',(-0.155778366559592,5.87990317054179E-5,-0.81900562256037));
#33603=CARTESIAN_POINT('',(-0.15535840277364,9.73258243413475E-5,-0.805194377439629));
#33604=CARTESIAN_POINT('',(-0.15555,-7.70311135908521E-15,-1.69400562256037));
#33605=CARTESIAN_POINT('Ctrl Pts',(-0.155778366559592,5.8799031705413E-5,
-0.81900562256037));
#33606=CARTESIAN_POINT('Ctrl Pts',(-0.155544814787508,-0.0482134994294573,
-0.815533999533272));
#33607=CARTESIAN_POINT('Ctrl Pts',(-0.105538280033678,-0.148433709770403,
-0.808356448827152));
#33608=CARTESIAN_POINT('Ctrl Pts',(0.0651130668400682,-0.171959437148373,
-0.797472970442005));
#33609=CARTESIAN_POINT('Ctrl Pts',(0.179800319818854,-0.0384916158499819,
-0.786355187404933));
#33610=CARTESIAN_POINT('Ctrl Pts',(0.129805978528337,0.130231207611715,
-0.775237404367861));
#33611=CARTESIAN_POINT('Ctrl Pts',(-0.039079449893004,0.179673470756717,
-0.764119621330788));
#33612=CARTESIAN_POINT('Ctrl Pts',(-0.143753821336814,0.0891312796984386,
-0.755375694061625));
#33613=CARTESIAN_POINT('Ctrl Pts',(-0.155492081597284,0.0187528760540667,
-0.750337694471485));
#33614=CARTESIAN_POINT('Ctrl Pts',(-0.155374470604174,0.000106635008702186,
-0.74900562256037));
#33615=CARTESIAN_POINT('Ctrl Pts',(-0.15535840277364,9.73258243413457E-5,
-0.805194377439629));
#33616=CARTESIAN_POINT('Ctrl Pts',(-0.155172926064984,-0.0323375807199177,
-0.802877855824775));
#33617=CARTESIAN_POINT('Ctrl Pts',(-0.129424084682119,-0.116930873012904,
-0.796855406530896));
#33618=CARTESIAN_POINT('Ctrl Pts',(0.00935975675220263,-0.183635922810792,
-0.787127029557995));
#33619=CARTESIAN_POINT('Ctrl Pts',(0.159391965553992,-0.0916731067972864,
-0.776009246520922));
#33620=CARTESIAN_POINT('Ctrl Pts',(0.163434873404623,0.0842543728731427,
-0.76489146348385));
#33621=CARTESIAN_POINT('Ctrl Pts',(0.0177855252092632,0.183012109670541,
-0.753773680446777));
#33622=CARTESIAN_POINT('Ctrl Pts',(-0.126401704041202,0.121695716778875,
-0.743874651765371));
#33623=CARTESIAN_POINT('Ctrl Pts',(-0.155154888799535,0.0346726790396201,
-0.737681550762988));
#33624=CARTESIAN_POINT('Ctrl Pts',(-0.15541051600741,-0.000122268189293732,
-0.735194377439629));
#33625=CARTESIAN_POINT('Origin',(0.,0.,-1.69400562256037));
#33626=CARTESIAN_POINT('',(-0.155549735916814,-0.000142332827097759,-0.88900562256037));
#33627=CARTESIAN_POINT('',(-0.155764687078297,7.18096733227647E-5,-0.875194377439629));
#33628=CARTESIAN_POINT('',(-0.15555,-7.70311135908521E-15,-1.69400562256037));
#33629=CARTESIAN_POINT('Ctrl Pts',(-0.155549735916814,-0.00014233282709776,
-0.88900562256037));
#33630=CARTESIAN_POINT('Ctrl Pts',(-0.155660546006807,-0.0121945460934811,
-0.888142159953108));
#33631=CARTESIAN_POINT('Ctrl Pts',(-0.148873723913168,-0.0758506683039087,
-0.883572769666822));
#33632=CARTESIAN_POINT('Ctrl Pts',(-0.0613810315003473,-0.173326652508083,
-0.875297451701512));
#33633=CARTESIAN_POINT('Ctrl Pts',(0.112384007026421,-0.145532108011909,
-0.86417966866444));
#33634=CARTESIAN_POINT('Ctrl Pts',(0.183214982554139,0.0155573026386719,
-0.853061885627367));
#33635=CARTESIAN_POINT('Ctrl Pts',(0.086236827089008,0.162397565102822,
-0.841944102590294));
#33636=CARTESIAN_POINT('Ctrl Pts',(-0.0897268284244655,0.160495656510048,
-0.830826319553223));
#33637=CARTESIAN_POINT('Ctrl Pts',(-0.154224330533382,0.0580895164678045,
-0.823180159543247));
#33638=CARTESIAN_POINT('Ctrl Pts',(-0.155794129292538,0.00331676339026758,
-0.819239927212296));
#33639=CARTESIAN_POINT('Ctrl Pts',(-0.155778366559592,5.8799031705413E-5,
-0.81900562256037));
#33640=CARTESIAN_POINT('Ctrl Pts',(-0.155764687078297,7.18096733227586E-5,
-0.875194377439629));
#33641=CARTESIAN_POINT('Ctrl Pts',(-0.155492443796488,-0.0474143206243747,
-0.871780088565587));
#33642=CARTESIAN_POINT('Ctrl Pts',(-0.106920290789132,-0.146924481715035,
-0.864659872012519));
#33643=CARTESIAN_POINT('Ctrl Pts',(0.0624505448146294,-0.172944172048056,
-0.853833727780429));
#33644=CARTESIAN_POINT('Ctrl Pts',(0.179184640777123,-0.0412628368220751,
-0.842715944743356));
#33645=CARTESIAN_POINT('Ctrl Pts',(0.131801051401358,0.128211700099984,
-0.831598161706284));
#33646=CARTESIAN_POINT('Ctrl Pts',(-0.0363009398827759,0.180255371505702,
-0.820480378669211));
#33647=CARTESIAN_POINT('Ctrl Pts',(-0.143056085809257,0.090756946949155,
-0.811679117246994));
#33648=CARTESIAN_POINT('Ctrl Pts',(-0.155469648212542,0.0195511722958854,
-0.806583783503799));
#33649=CARTESIAN_POINT('Ctrl Pts',(-0.15535840277364,9.73258243413457E-5,
-0.805194377439629));
#33650=CARTESIAN_POINT('Origin',(0.,0.,-1.69400562256037));
#33651=CARTESIAN_POINT('',(-0.155297992403489,2.48232510734268E-5,-0.95900562256037));
#33652=CARTESIAN_POINT('',(-0.155574065889681,-0.000140958060374008,-0.94519437743963));
#33653=CARTESIAN_POINT('',(-0.15555,-7.70311135908521E-15,-1.69400562256037));
#33654=CARTESIAN_POINT('Ctrl Pts',(-0.155297992403489,2.48232510734348E-5,
-0.95900562256037));
#33655=CARTESIAN_POINT('Ctrl Pts',(-0.155258843021101,-0.027462174823301,
-0.95704439269392));
#33656=CARTESIAN_POINT('Ctrl Pts',(-0.135189599997863,-0.106941847650722,
-0.951377235148446));
#33657=CARTESIAN_POINT('Ctrl Pts',(-0.00822520867957112,-0.183690243180965,
-0.942004149923946));
#33658=CARTESIAN_POINT('Ctrl Pts',(0.14990580454341,-0.106480088570106,
-0.930886366886874));
#33659=CARTESIAN_POINT('Ctrl Pts',(0.170736022599271,0.0682566486482162,
-0.919768583849802));
#33660=CARTESIAN_POINT('Ctrl Pts',(0.0351867613017287,0.18047617938886,
-0.908650800812729));
#33661=CARTESIAN_POINT('Ctrl Pts',(-0.119560116328767,0.13151762975358,
-0.898396480382919));
#33662=CARTESIAN_POINT('Ctrl Pts',(-0.155184956008855,0.0395328018678041,
-0.891848087632132));
#33663=CARTESIAN_POINT('Ctrl Pts',(-0.155549735916814,-0.00014233282709776,
-0.88900562256037));
#33664=CARTESIAN_POINT('Ctrl Pts',(-0.155574065889681,-0.000140958060374001,
-0.94519437743963));
#33665=CARTESIAN_POINT('Ctrl Pts',(-0.155678059406658,-0.0113883944085503,
-0.944388248985422));
#33666=CARTESIAN_POINT('Ctrl Pts',(-0.149431301112879,-0.0742278940490436,
-0.939876192852191));
#33667=CARTESIAN_POINT('Ctrl Pts',(-0.0640495814302482,-0.172358371748057,
-0.931658209039936));
#33668=CARTESIAN_POINT('Ctrl Pts',(0.110123842548254,-0.147249775875683,
-0.920540426002863));
#33669=CARTESIAN_POINT('Ctrl Pts',(0.183433319364821,0.0127269218523267,
-0.909422642965792));
#33670=CARTESIAN_POINT('Ctrl Pts',(0.0887336874904625,0.161046856216992,
-0.898304859928718));
#33671=CARTESIAN_POINT('Ctrl Pts',(-0.0872383533320315,0.16186175243382,
-0.887187076891646));
#33672=CARTESIAN_POINT('Ctrl Pts',(-0.153804569176776,0.0597032248363634,
-0.879483582728616));
#33673=CARTESIAN_POINT('Ctrl Pts',(-0.155787941321947,0.00412793931088879,
-0.875486016244611));
#33674=CARTESIAN_POINT('Ctrl Pts',(-0.155764687078297,7.18096733227586E-5,
-0.875194377439629));
#33675=CARTESIAN_POINT('Origin',(0.,0.,-1.69400562256037));
#33676=CARTESIAN_POINT('',(-0.15564091233498,0.000130139906504897,-1.02900562256037));
#33677=CARTESIAN_POINT('',(-0.155295176870621,1.17227753446275E-5,-1.01519437743963));
#33678=CARTESIAN_POINT('',(-0.15555,-7.70311135908521E-15,-1.69400562256037));
#33679=CARTESIAN_POINT('Ctrl Pts',(-0.15564091233498,0.00013013990650489,
-1.02900562256037));
#33680=CARTESIAN_POINT('Ctrl Pts',(-0.155258831108901,-0.0425030626805927,
-1.02594662543473));
#33681=CARTESIAN_POINT('Ctrl Pts',(-0.115015154867651,-0.137419804614315,
-1.01918170063007));
#33682=CARTESIAN_POINT('Ctrl Pts',(0.0456441385565052,-0.178118983022976,
-1.00871084814638));
#33683=CARTESIAN_POINT('Ctrl Pts',(0.174423500194588,-0.0581910824574806,
-0.997593065109308));
#33684=CARTESIAN_POINT('Ctrl Pts',(0.143445970860419,0.11503483360103,-0.986475282072236));
#33685=CARTESIAN_POINT('Ctrl Pts',(-0.0189157028212204,0.182898758017883,
-0.975357499035165));
#33686=CARTESIAN_POINT('Ctrl Pts',(-0.138367090429786,0.100822903310039,
-0.966200945864541));
#33687=CARTESIAN_POINT('Ctrl Pts',(-0.155332819448999,0.0244770846789348,
-0.960750320372944));
#33688=CARTESIAN_POINT('Ctrl Pts',(-0.155297992403489,2.48232510734348E-5,
-0.95900562256037));
#33689=CARTESIAN_POINT('Ctrl Pts',(-0.155295176870621,1.1722775344624E-5,
-1.01519437743963));
#33690=CARTESIAN_POINT('Ctrl Pts',(-0.155277247152915,-0.026672930115448,
-1.01329048172623));
#33691=CARTESIAN_POINT('Ctrl Pts',(-0.136055195927886,-0.105323398094664,
-1.00768065833381));
#33692=CARTESIAN_POINT('Ctrl Pts',(-0.0110600915264488,-0.183541362009925,
-0.99836490726237));
#33693=CARTESIAN_POINT('Ctrl Pts',(0.148244063463316,-0.10878168430814,
-0.987247124225296));
#33694=CARTESIAN_POINT('Ctrl Pts',(0.171769434874196,0.0656126393009093,
-0.976129341188226));
#33695=CARTESIAN_POINT('Ctrl Pts',(0.0379688103673882,0.17991144108232,
-0.965011558151151));
#33696=CARTESIAN_POINT('Ctrl Pts',(-0.118384802577525,0.133087407394055,
-0.954699903568288));
#33697=CARTESIAN_POINT('Ctrl Pts',(-0.155199981190967,0.0403182355500233,
-0.948094176664447));
#33698=CARTESIAN_POINT('Ctrl Pts',(-0.155574065889681,-0.000140958060374001,
-0.94519437743963));
#33699=CARTESIAN_POINT('Origin',(0.,0.,-1.69400562256037));
#33700=CARTESIAN_POINT('',(-0.155715979727104,-0.000103239153171051,-1.09900562256037));
#33701=CARTESIAN_POINT('',(-0.15561713819096,0.000135214911208083,-1.08519437743963));
#33702=CARTESIAN_POINT('',(-0.15555,-7.70311135908521E-15,-1.69400562256037));
#33703=CARTESIAN_POINT('Ctrl Pts',(-0.155715979727104,-0.000103239153171026,
-1.09900562256037));
#33704=CARTESIAN_POINT('Ctrl Pts',(-0.155764022106253,-0.0063786663684298,
-1.09855478585457));
#33705=CARTESIAN_POINT('Ctrl Pts',(-0.15256950177487,-0.0641894789869248,
-1.09439802146974));
#33706=CARTESIAN_POINT('Ctrl Pts',(-0.0802215287029169,-0.165451702409712,
-1.08653532940589));
#33707=CARTESIAN_POINT('Ctrl Pts',(0.0955539257930597,-0.157096170428305,
-1.07541754636882));
#33708=CARTESIAN_POINT('Ctrl Pts',(0.183810220956364,-0.00485408793464279,
-1.06429976333174));
#33709=CARTESIAN_POINT('Ctrl Pts',(0.103712198059592,0.151833920687547,
-1.05318198029467));
#33710=CARTESIAN_POINT('Ctrl Pts',(-0.0713772583275903,0.169455145957098,
-1.0420641972576));
#33711=CARTESIAN_POINT('Ctrl Pts',(-0.150904081293975,0.0697258462719453,
-1.03400541134617));
#33712=CARTESIAN_POINT('Ctrl Pts',(-0.1557217166015,0.0091464024950112,
-1.02965255311376));
#33713=CARTESIAN_POINT('Ctrl Pts',(-0.15564091233498,0.00013013990650489,
-1.02900562256037));
#33714=CARTESIAN_POINT('Ctrl Pts',(-0.15561713819096,0.000135214911208083,
-1.08519437743963));
#33715=CARTESIAN_POINT('Ctrl Pts',(-0.155234629029245,-0.0417154247154185,
-1.08219271446705));
#33716=CARTESIAN_POINT('Ctrl Pts',(-0.116246810649056,-0.135864191994095,
-1.07548512381544));
#33717=CARTESIAN_POINT('Ctrl Pts',(0.0428888445928814,-0.17880241665738,
-1.06507160548481));
#33718=CARTESIAN_POINT('Ctrl Pts',(0.173504336038483,-0.060876946119833,
-1.05395382244773));
#33719=CARTESIAN_POINT('Ctrl Pts',(0.145204811647398,0.112806559505532,
-1.04283603941066));
#33720=CARTESIAN_POINT('Ctrl Pts',(-0.0160898036409584,0.183168980484762,
-1.03171825637359));
#33721=CARTESIAN_POINT('Ctrl Pts',(-0.13754985709603,0.102444722253558,
-1.02250436904991));
#33722=CARTESIAN_POINT('Ctrl Pts',(-0.155312147298262,0.0252686720728152,
-1.01699640940526));
#33723=CARTESIAN_POINT('Ctrl Pts',(-0.155295176870621,1.1722775344624E-5,
-1.01519437743963));
#33724=CARTESIAN_POINT('Origin',(0.,0.,-1.69400562256037));
#33725=CARTESIAN_POINT('',(-0.155322542976565,-6.74140301452986E-5,-1.16900562256037));
#33726=CARTESIAN_POINT('',(-0.155735118268745,-9.28043970148673E-5,-1.15519437743963));
#33727=CARTESIAN_POINT('',(-0.15555,-7.70311135908521E-15,-1.69400562256037));
#33728=CARTESIAN_POINT('Ctrl Pts',(-0.155322542976565,-6.74140301453116E-5,
-1.16900562256037));
#33729=CARTESIAN_POINT('Ctrl Pts',(-0.15540725279883,-0.021762817988561,
-1.16745701859538));
#33730=CARTESIAN_POINT('Ctrl Pts',(-0.141033818316528,-0.0952697082468468,
-1.16220248695136));
#33731=CARTESIAN_POINT('Ctrl Pts',(-0.0285426415962272,-0.181645470927358,
-1.15324202762832));
#33732=CARTESIAN_POINT('Ctrl Pts',(0.137174554457832,-0.122445502600127,
-1.14212424459125));
#33733=CARTESIAN_POINT('Ctrl Pts',(0.177251682996677,0.0489039913764663,
-1.13100646155418));
#33734=CARTESIAN_POINT('Ctrl Pts',(0.0549815489042986,0.175461644748333,
-1.11988867851711));
#33735=CARTESIAN_POINT('Ctrl Pts',(-0.110646694549052,0.142696374884672,
-1.10922173218584));
#33736=CARTESIAN_POINT('Ctrl Pts',(-0.155369108426059,0.0452060407225295,
-1.10226071353359));
#33737=CARTESIAN_POINT('Ctrl Pts',(-0.155715979727104,-0.000103239153171026,
-1.09900562256037));
#33738=CARTESIAN_POINT('Ctrl Pts',(-0.155735118268745,-9.28043970148612E-5,
-1.15519437743963));
#33739=CARTESIAN_POINT('Ctrl Pts',(-0.155773755432419,-0.00556840185665671,
-1.15480087488688));
#33740=CARTESIAN_POINT('Ctrl Pts',(-0.153026196109622,-0.0625728674990446,
-1.15070144465511));
#33741=CARTESIAN_POINT('Ctrl Pts',(-0.0827662568575337,-0.164193495360887,
-1.14289608674431));
#33742=CARTESIAN_POINT('Ctrl Pts',(0.0931172382976506,-0.158552632033813,
-1.13177830370724));
#33743=CARTESIAN_POINT('Ctrl Pts',(0.183713369824886,-0.00769122491000194,
-1.12066052067017));
#33744=CARTESIAN_POINT('Ctrl Pts',(0.106043890579969,0.150214681252184,
-1.10954273763309));
#33745=CARTESIAN_POINT('Ctrl Pts',(-0.0687526515134619,0.170536887807008,
-1.09842495459602));
#33746=CARTESIAN_POINT('Ctrl Pts',(-0.150386323062114,0.0713465315647904,
-1.09030883453153));
#33747=CARTESIAN_POINT('Ctrl Pts',(-0.155706884343325,0.00995441470151274,
-1.08589864214607));
#33748=CARTESIAN_POINT('Ctrl Pts',(-0.15561713819096,0.000135214911208083,
-1.08519437743963));
#33749=CARTESIAN_POINT('Origin',(0.,0.,-1.69400562256037));
#33750=CARTESIAN_POINT('',(-0.155469168273574,0.00013710264519145,-1.23900562256037));
#33751=CARTESIAN_POINT('',(-0.155333899255999,-7.87989482575052E-5,-1.22519437743963));
#33752=CARTESIAN_POINT('',(-0.15555,-7.70311135908521E-15,-1.69400562256037));
#33753=CARTESIAN_POINT('Ctrl Pts',(-0.155469168273574,0.000137102645191454,
-1.23900562256037));
#33754=CARTESIAN_POINT('Ctrl Pts',(-0.155155856663809,-0.0368497007893972,
-1.23635925133619));
#33755=CARTESIAN_POINT('Ctrl Pts',(-0.12342921310041,-0.126115115492115,
-1.23000695243298));
#33756=CARTESIAN_POINT('Ctrl Pts',(0.0256122765083437,-0.182081769516105,
-1.21994872585076));
#33757=CARTESIAN_POINT('Ctrl Pts',(0.166895497950393,-0.0771728725754398,
-1.20883094281368));
#33758=CARTESIAN_POINT('Ctrl Pts',(0.155316829566065,0.0984197233850115,
-1.19771315977661));
#33759=CARTESIAN_POINT('Ctrl Pts',(0.00148133352129465,0.183868336449635,
-1.18659537673954));
#33760=CARTESIAN_POINT('Ctrl Pts',(-0.132094093876729,0.112464811996422,
-1.17702619766746));
#33761=CARTESIAN_POINT('Ctrl Pts',(-0.155204535718084,0.030155942297909,
-1.1711629462744));
#33762=CARTESIAN_POINT('Ctrl Pts',(-0.155322542976565,-6.74140301453116E-5,
-1.16900562256037));
#33763=CARTESIAN_POINT('Ctrl Pts',(-0.155333899255999,-7.87989482575243E-5,
-1.22519437743963));
#33764=CARTESIAN_POINT('Ctrl Pts',(-0.155429657836139,-0.0209671487471519,
-1.22370310762769));
#33765=CARTESIAN_POINT('Ctrl Pts',(-0.141776642167995,-0.0936447578516373,
-1.21850591013673));
#33766=CARTESIAN_POINT('Ctrl Pts',(-0.0313435345808448,-0.181183167079792,
-1.20960278496674));
#33767=CARTESIAN_POINT('Ctrl Pts',(0.135267852386276,-0.124548646334775,
-1.19848500192967));
#33768=CARTESIAN_POINT('Ctrl Pts',(0.177985546579018,0.0461616984305375,
-1.1873672188926));
#33769=CARTESIAN_POINT('Ctrl Pts',(0.0576838223577768,0.174591906545624,
-1.17624943585553));
#33770=CARTESIAN_POINT('Ctrl Pts',(-0.109323369976581,0.144225213236364,
-1.1655251553712));
#33771=CARTESIAN_POINT('Ctrl Pts',(-0.155409878417394,0.0459996706834923,
-1.1585068025659));
#33772=CARTESIAN_POINT('Ctrl Pts',(-0.155735118268745,-9.28043970148612E-5,
-1.15519437743963));
#33773=CARTESIAN_POINT('Origin',(0.,0.,-1.69400562256037));
#33774=CARTESIAN_POINT('',(-0.155804675564127,-9.9298664568263E-6,-1.30900562256037));
#33775=CARTESIAN_POINT('',(-0.155447125224745,0.0001327912984651,-1.29519437743963));
#33776=CARTESIAN_POINT('',(-0.15555,-7.70311135908521E-15,-1.69400562256037));
#33777=CARTESIAN_POINT('Ctrl Pts',(-0.155804675564127,-9.92986645682631E-6,
-1.30900562256037));
#33778=CARTESIAN_POINT('Ctrl Pts',(-0.155805165222731,-0.000541004492398835,
-1.30896741175602));
#33779=CARTESIAN_POINT('Ctrl Pts',(-0.155562120987005,-0.0525786248856173,
-1.30522327327266));
#33780=CARTESIAN_POINT('Ctrl Pts',(-0.0980726456853608,-0.155536219688844,
-1.29777320711026));
#33781=CARTESIAN_POINT('Ctrl Pts',(0.0775453683472552,-0.166722749977294,
-1.28665542407319));
#33782=CARTESIAN_POINT('Ctrl Pts',(0.18213850936899,-0.025205612527195,
-1.27553764103612));
#33783=CARTESIAN_POINT('Ctrl Pts',(0.119908476028974,0.139397693201698,
-1.26441985799905));
#33784=CARTESIAN_POINT('Ctrl Pts',(-0.0521473853035587,0.176324728004856,
-1.25330207496197));
#33785=CARTESIAN_POINT('Ctrl Pts',(-0.146855130761894,0.0814052574977526,
-1.24483066314908));
#33786=CARTESIAN_POINT('Ctrl Pts',(-0.155594612253418,0.0149459117665484,
-1.24006517901521));
#33787=CARTESIAN_POINT('Ctrl Pts',(-0.155469168273574,0.000137102645191454,
-1.23900562256037));
#33788=CARTESIAN_POINT('Ctrl Pts',(-0.155447125224745,0.000132791298465095,
-1.29519437743963));
#33789=CARTESIAN_POINT('Ctrl Pts',(-0.155153338736769,-0.0360656743444678,
-1.2926053403685));
#33790=CARTESIAN_POINT('Ctrl Pts',(-0.124516957166434,-0.124526645405497,
-1.28631037561835));
#33791=CARTESIAN_POINT('Ctrl Pts',(0.0227981919227724,-0.182455473034852,
-1.27630948318918));
#33792=CARTESIAN_POINT('Ctrl Pts',(0.165684184825268,-0.0797402538976839,
-1.26519170015211));
#33793=CARTESIAN_POINT('Ctrl Pts',(0.1568177463056,0.0960101642333705,-1.25407391711503));
#33794=CARTESIAN_POINT('Ctrl Pts',(0.00431976977229057,0.183823547954278,
-1.24295613407796));
#33795=CARTESIAN_POINT('Ctrl Pts',(-0.13114891460843,0.114075301211355,
-1.23332962085283));
#33796=CARTESIAN_POINT('Ctrl Pts',(-0.155191689917924,0.0309421121184549,
-1.22740903530672));
#33797=CARTESIAN_POINT('Ctrl Pts',(-0.155333899255999,-7.87989482575243E-5,
-1.22519437743963));
#33798=CARTESIAN_POINT('Origin',(0.,0.,-1.69400562256037));
#33799=CARTESIAN_POINT('',(-0.155440006104157,-0.000131091492392236,-1.37900562256037));
#33800=CARTESIAN_POINT('',(-0.155805262673826,4.97304114227787E-6,-1.36519437743963));
#33801=CARTESIAN_POINT('',(-0.15555,-7.70311135908521E-15,-1.69400562256037));
#33802=CARTESIAN_POINT('Ctrl Pts',(-0.155440006104157,-0.000131091492392219,
-1.37900562256037));
#33803=CARTESIAN_POINT('Ctrl Pts',(-0.155566842076363,-0.0160155424259783,
-1.37786964449684));
#33804=CARTESIAN_POINT('Ctrl Pts',(-0.14602074484413,-0.0835713921170919,
-1.37302773875428));
#33805=CARTESIAN_POINT('Ctrl Pts',(-0.048508054493723,-0.177360442508133,
-1.3644799053327));
#33806=CARTESIAN_POINT('Ctrl Pts',(0.12275151636726,-0.136900786130964,
-1.35336212229563));
#33807=CARTESIAN_POINT('Ctrl Pts',(0.181581280715027,0.0289481974204555,
-1.34224433925855));
#33808=CARTESIAN_POINT('Ctrl Pts',(0.0740982434113141,0.1682831233296,-1.33112655622148));
#33809=CARTESIAN_POINT('Ctrl Pts',(-0.100649733124876,0.15353607539823,
-1.32004698398875));
#33810=CARTESIAN_POINT('Ctrl Pts',(-0.155757675006093,0.0509660022204176,
-1.31267333943505));
#33811=CARTESIAN_POINT('Ctrl Pts',(-0.155804675564127,-9.92986645682631E-6,
-1.30900562256037));
#33812=CARTESIAN_POINT('Ctrl Pts',(-0.155805262673826,4.97304114227722E-6,
-1.36519437743963));
#33813=CARTESIAN_POINT('Ctrl Pts',(-0.155781279836539,-0.0512357195429724,
-1.36150757310931));
#33814=CARTESIAN_POINT('Ctrl Pts',(-0.100160425534363,-0.154027506270637,
-1.35411484109998));
#33815=CARTESIAN_POINT('Ctrl Pts',(0.0749622096468331,-0.167900042901071,
-1.34301618141161));
#33816=CARTESIAN_POINT('Ctrl Pts',(0.181727664822887,-0.0280145148561602,
-1.33189839837454));
#33817=CARTESIAN_POINT('Ctrl Pts',(0.122046243641521,0.137529893387063,
-1.32078061533747));
#33818=CARTESIAN_POINT('Ctrl Pts',(-0.0494190162937222,0.17710877458793,
-1.3096628323004));
#33819=CARTESIAN_POINT('Ctrl Pts',(-0.146231685180962,0.0830303065190035,
-1.30113408633445));
#33820=CARTESIAN_POINT('Ctrl Pts',(-0.155573862447942,0.01574852996355,
-1.29631126804753));
#33821=CARTESIAN_POINT('Ctrl Pts',(-0.155447125224745,0.000132791298465095,
-1.29519437743963));
#33822=CARTESIAN_POINT('Origin',(0.,0.,-1.69400562256037));
#33823=CARTESIAN_POINT('',(-0.155338051549543,8.26344013249621E-5,-1.44900562256037));
#33824=CARTESIAN_POINT('',(-0.15546172451378,-0.000135797342094887,-1.43519437743963));
#33825=CARTESIAN_POINT('',(-0.15555,-7.70311135908521E-15,-1.69400562256037));
#33826=CARTESIAN_POINT('Ctrl Pts',(-0.155338051549543,8.26344013249731E-5,
-1.44900562256037));
#33827=CARTESIAN_POINT('Ctrl Pts',(-0.155187751699248,-0.0312036093690435,
-1.44677187723765));
#33828=CARTESIAN_POINT('Ctrl Pts',(-0.130830226648687,-0.114611274732386,
-1.4408322042359));
#33829=CARTESIAN_POINT('Ctrl Pts',(0.00526457092671344,-0.183798721027812,
-1.43118660355513));
#33830=CARTESIAN_POINT('Ctrl Pts',(0.157309138173746,-0.095202988083288,
-1.42006882051806));
#33831=CARTESIAN_POINT('Ctrl Pts',(0.165272159879762,0.0805908485969487,
-1.40895103748099));
#33832=CARTESIAN_POINT('Ctrl Pts',(0.021860095314849,0.182570218824516,
-1.39783325444391));
#33833=CARTESIAN_POINT('Ctrl Pts',(-0.124874771184232,0.123997024126219,
-1.38785144947038));
#33834=CARTESIAN_POINT('Ctrl Pts',(-0.155153062131851,0.0358046715997731,
-1.38157557217586));
#33835=CARTESIAN_POINT('Ctrl Pts',(-0.155440006104157,-0.000131091492392219,
-1.37900562256037));
#33836=CARTESIAN_POINT('Ctrl Pts',(-0.15546172451378,-0.000135797342094889,
-1.43519437743963));
#33837=CARTESIAN_POINT('Ctrl Pts',(-0.155587764885392,-0.015213215124397,
-1.43411573352915));
#33838=CARTESIAN_POINT('Ctrl Pts',(-0.146649276514878,-0.0819462556503598,
-1.42933116193965));
#33839=CARTESIAN_POINT('Ctrl Pts',(-0.0512404048426255,-0.176590393721669,
-1.42084066267112));
#33840=CARTESIAN_POINT('Ctrl Pts',(0.120623364083146,-0.138779552138408,
-1.40972287963405));
#33841=CARTESIAN_POINT('Ctrl Pts',(0.1820065472977,0.0261414484512927,-1.39860509659698));
#33842=CARTESIAN_POINT('Ctrl Pts',(0.0766874125244866,0.167119108331645,
-1.3874873135599));
#33843=CARTESIAN_POINT('Ctrl Pts',(-0.0988707767058873,0.15503008489993,
-1.37636953052283));
#33844=CARTESIAN_POINT('Ctrl Pts',(-0.155684373061444,0.0520429010369321,
-1.36893855181607));
#33845=CARTESIAN_POINT('Ctrl Pts',(-0.155805387072118,0.000270757049356713,
-1.36521350078834));
#33846=CARTESIAN_POINT('Ctrl Pts',(-0.155805262673826,4.97304114227722E-6,
-1.36519437743963));
#33847=CARTESIAN_POINT('Origin',(0.,0.,-1.69400562256037));
#33848=CARTESIAN_POINT('',(-0.155739242772632,9.98782012467415E-5,-1.51900562256037));
#33849=CARTESIAN_POINT('',(-0.155325699155423,7.24743171157949E-5,-1.50519437743963));
#33850=CARTESIAN_POINT('',(-0.15555,-7.70311135908521E-15,-1.69400562256037));
#33851=CARTESIAN_POINT('Ctrl Pts',(-0.155739242772632,9.98782012467418E-5,
-1.51900562256037));
#33852=CARTESIAN_POINT('Ctrl Pts',(-0.155421972044204,-0.0462505870687982,
-1.51567410997846));
#33853=CARTESIAN_POINT('Ctrl Pts',(-0.108881181232048,-0.144750054452956,
-1.50863666971753));
#33854=CARTESIAN_POINT('Ctrl Pts',(0.0585821121664253,-0.174283509875506,
-1.49789330177756));
#33855=CARTESIAN_POINT('Ctrl Pts',(0.178219584548083,-0.0452513232337437,
-1.4867755187405));
#33856=CARTESIAN_POINT('Ctrl Pts',(0.134626373349144,0.125244912864161,
-1.47565773570342));
#33857=CARTESIAN_POINT('Ctrl Pts',(-0.0322746164076941,0.18101828554357,
-1.46453995266635));
#33858=CARTESIAN_POINT('Ctrl Pts',(-0.14202024933615,0.0931040090647467,
-1.455655914952));
#33859=CARTESIAN_POINT('Ctrl Pts',(-0.155437108852768,0.0207022885781798,
-1.45047780491667));
#33860=CARTESIAN_POINT('Ctrl Pts',(-0.155338051549543,8.26344013249731E-5,
-1.44900562256037));
#33861=CARTESIAN_POINT('Ctrl Pts',(-0.155325699155423,7.24743171158018E-5,
-1.50519437743963));
#33862=CARTESIAN_POINT('Ctrl Pts',(-0.155199852209928,-0.0304170665609612,
-1.50301796626996));
#33863=CARTESIAN_POINT('Ctrl Pts',(-0.131782164237154,-0.113003219889635,
-1.49713562742127));
#33864=CARTESIAN_POINT('Ctrl Pts',(0.00242683334840427,-0.183856950102903,
-1.48754736089355));
#33865=CARTESIAN_POINT('Ctrl Pts',(0.155820388725155,-0.0976208199140973,
-1.47642957785648));
#33866=CARTESIAN_POINT('Ctrl Pts',(0.166496760685316,0.078030035232174,
-1.46531179481941));
#33867=CARTESIAN_POINT('Ctrl Pts',(0.0246759993484255,0.182210807009283,
-1.45419401178234));
#33868=CARTESIAN_POINT('Ctrl Pts',(-0.123793478086846,0.125586772778578,
-1.44415487265574));
#33869=CARTESIAN_POINT('Ctrl Pts',(-0.155154724382133,0.036588699617641,
-1.43782166120817));
#33870=CARTESIAN_POINT('Ctrl Pts',(-0.15546172451378,-0.000135797342094889,
-1.43519437743963));
#33871=CARTESIAN_POINT('Origin',(2.59090492670967E-17,0.,-0.02));
#33872=CARTESIAN_POINT('',(0.00853826423429785,0.19521336543348,-0.02));
#33873=CARTESIAN_POINT('Ctrl Pts',(0.133821766704343,-0.0798002879704671,
-0.0200000000000001));
#33874=CARTESIAN_POINT('Ctrl Pts',(0.136065138599399,-0.0769506293259119,
-0.0200000000000001));
#33875=CARTESIAN_POINT('Ctrl Pts',(0.138197889310311,-0.0740223739865894,
-0.0199999999999998));
#33876=CARTESIAN_POINT('Ctrl Pts',(0.140214087153587,-0.0710196745109591,
-0.0199999999999999));
#33877=CARTESIAN_POINT('Ctrl Pts',(0.145120054681607,-0.0637132754028678,
-0.0199999999999999));
#33878=CARTESIAN_POINT('Ctrl Pts',(0.149337231868511,-0.055967386575868,
-0.0200000000000001));
#33879=CARTESIAN_POINT('Ctrl Pts',(0.152881379977793,-0.0478854058222795,
-0.0199999999999998));
#33880=CARTESIAN_POINT('Ctrl Pts',(0.154570678326317,-0.0440331749563981,
-0.0199999999999997));
#33881=CARTESIAN_POINT('Ctrl Pts',(0.156106559607416,-0.0401039093554644,
-0.0199999999999995));
#33882=CARTESIAN_POINT('Ctrl Pts',(0.157485311894354,-0.036122580876755,
-0.0199999999999995));
#33883=CARTESIAN_POINT('Ctrl Pts',(0.160039385365418,-0.0287473579716647,
-0.0199999999999996));
#33884=CARTESIAN_POINT('Ctrl Pts',(0.162060174255282,-0.0211826817802034,
-0.0199999999999997));
#33885=CARTESIAN_POINT('Ctrl Pts',(0.163555878906819,-0.0134954408667204,
-0.0199999999999998));
#33886=CARTESIAN_POINT('Ctrl Pts',(0.164335346674248,-0.00948933143437693,
-0.0199999999999998));
#33887=CARTESIAN_POINT('Ctrl Pts',(0.164972230950227,-0.00544823120734308,
-0.0200000000000002));
#33888=CARTESIAN_POINT('Ctrl Pts',(0.165465981759546,-0.00138582933311573,
-0.0200000000000002));
#33889=CARTESIAN_POINT('Ctrl Pts',(0.166873155854188,0.0101918867365069,
-0.0200000000000002));
#33890=CARTESIAN_POINT('Ctrl Pts',(0.167113372873192,0.0218697098856196,
-0.0199999999999994));
#33891=CARTESIAN_POINT('Ctrl Pts',(0.166212385384324,0.0334410544872706,
-0.0199999999999993));
#33892=CARTESIAN_POINT('Ctrl Pts',(0.165524991089037,0.0422692306453721,
-0.0199999999999993));
#33893=CARTESIAN_POINT('Ctrl Pts',(0.164172506243096,0.051036511458747,
-0.0199999999999997));
#33894=CARTESIAN_POINT('Ctrl Pts',(0.162147313208725,0.0596568175050613,
-0.0199999999999997));
#33895=CARTESIAN_POINT('Ctrl Pts',(0.161339114894091,0.0630969423228057,
-0.0199999999999997));
#33896=CARTESIAN_POINT('Ctrl Pts',(0.160423339052115,0.066513402035509,
-0.0199999999999997));
#33897=CARTESIAN_POINT('Ctrl Pts',(0.159403754602336,0.069887176638175,
-0.0199999999999997));
#33898=CARTESIAN_POINT('Ctrl Pts',(0.157419300482608,0.0764536762652955,
-0.0199999999999997));
#33899=CARTESIAN_POINT('Ctrl Pts',(0.155039126041078,0.0828715355915416,
-0.0199999999999998));
#33900=CARTESIAN_POINT('Ctrl Pts',(0.152264969414956,0.0891018848696017,
-0.0199999999999998));
#33901=CARTESIAN_POINT('Ctrl Pts',(0.149133055506545,0.0961357045805976,
-0.0199999999999998));
#33902=CARTESIAN_POINT('Ctrl Pts',(0.145499258844698,0.10293079067009,-0.0199999999999997));
#33903=CARTESIAN_POINT('Ctrl Pts',(0.141411895748059,0.109465395998025,
-0.0199999999999996));
#33904=CARTESIAN_POINT('Ctrl Pts',(0.138924049814933,0.113442799254188,
-0.0199999999999996));
#33905=CARTESIAN_POINT('Ctrl Pts',(0.136267962558613,0.117323661573993,
-0.0199999999999997));
#33906=CARTESIAN_POINT('Ctrl Pts',(0.133452844321485,0.121102461008537,
-0.0199999999999997));
#33907=CARTESIAN_POINT('Ctrl Pts',(0.131317154149409,0.123969248168011,
-0.0199999999999997));
#33908=CARTESIAN_POINT('Ctrl Pts',(0.129090064208231,0.126776619840538,
-0.0199999999999998));
#33909=CARTESIAN_POINT('Ctrl Pts',(0.126784735751445,0.129512001730073,
-0.0199999999999999));
#33910=CARTESIAN_POINT('Ctrl Pts',(0.119384017280744,0.138293306283324,
-0.0200000000000001));
#33911=CARTESIAN_POINT('Ctrl Pts',(0.111159161660068,0.146362743803953,
-0.0200000000000003));
#33912=CARTESIAN_POINT('Ctrl Pts',(0.102260233844386,0.153651749300115,
-0.0200000000000002));
#33913=CARTESIAN_POINT('Ctrl Pts',(0.0967966677903543,0.158126891004974,
-0.0200000000000001));
#33914=CARTESIAN_POINT('Ctrl Pts',(0.0910781750600193,0.162307627165175,
-0.0199999999999998));
#33915=CARTESIAN_POINT('Ctrl Pts',(0.0851331862206853,0.166174253363221,
-0.0199999999999996));
#33916=CARTESIAN_POINT('Ctrl Pts',(0.0806708967451739,0.169076530534058,
-0.0199999999999995));
#33917=CARTESIAN_POINT('Ctrl Pts',(0.0760753987718405,0.171804249124038,
-0.02));
#33918=CARTESIAN_POINT('Ctrl Pts',(0.0713880909719757,0.174332475493028,
-0.02));
#33919=CARTESIAN_POINT('Ctrl Pts',(0.0601005419700875,0.18042072065343,
-0.02));
#33920=CARTESIAN_POINT('Ctrl Pts',(0.0482596588054404,0.185373180166949,
-0.0199999999999998));
#33921=CARTESIAN_POINT('Ctrl Pts',(0.0360387384670489,0.189087621526514,
-0.0199999999999995));
#33922=CARTESIAN_POINT('Ctrl Pts',(0.0270584772457173,0.191817093021016,
-0.0199999999999992));
#33923=CARTESIAN_POINT('Ctrl Pts',(0.0178719156836204,0.19387762520946,
-0.02));
#33924=CARTESIAN_POINT('Ctrl Pts',(0.00853826423429785,0.19521336543348,
-0.02));
#33925=CARTESIAN_POINT('',(-0.1954,-2.39295984553393E-17,-0.02));
#33926=CARTESIAN_POINT('Origin',(0.,0.,-0.02));
#33927=CARTESIAN_POINT('',(-0.149577187126323,0.126230651412956,-0.0200000000000003));
#33928=CARTESIAN_POINT('Origin',(0.,0.,-0.02));
#33929=CARTESIAN_POINT('Ctrl Pts',(-0.149578925757925,0.126231591330479,
-0.0200000000000002));
#33930=CARTESIAN_POINT('Ctrl Pts',(-0.152148426341253,0.122532430052756,
-0.0200000000000002));
#33931=CARTESIAN_POINT('Ctrl Pts',(-0.154577059731215,0.118743491976515,
-0.0200000000000004));
#33932=CARTESIAN_POINT('Ctrl Pts',(-0.156856766744289,0.114867806158737,
-0.0200000000000003));
#33933=CARTESIAN_POINT('Ctrl Pts',(-0.161319559432387,0.107280698591954,
-0.0200000000000001));
#33934=CARTESIAN_POINT('Ctrl Pts',(-0.165212332552683,0.099361225354574,
-0.0200000000000002));
#33935=CARTESIAN_POINT('Ctrl Pts',(-0.168532013693597,0.0911785794352264,
-0.0200000000000004));
#33936=CARTESIAN_POINT('Ctrl Pts',(-0.17021136272293,0.0870391702875616,
-0.0200000000000005));
#33937=CARTESIAN_POINT('Ctrl Pts',(-0.171744680598151,0.0828297970998818,
-0.0200000000000001));
#33938=CARTESIAN_POINT('Ctrl Pts',(-0.173127719604902,0.0785680462167742,
-0.02));
#33939=CARTESIAN_POINT('Ctrl Pts',(-0.176934316037692,0.0668382499999685,
-0.02));
#33940=CARTESIAN_POINT('Ctrl Pts',(-0.179597768596154,0.05474203377193,
-0.02));
#33941=CARTESIAN_POINT('Ctrl Pts',(-0.18110253115427,0.042471584803998,
-0.0199999999999998));
#33942=CARTESIAN_POINT('Ctrl Pts',(-0.181600194320072,0.0384134359311063,
-0.0199999999999998));
#33943=CARTESIAN_POINT('Ctrl Pts',(-0.181970877474762,0.0343338115398897,
-0.0200000000000001));
#33944=CARTESIAN_POINT('Ctrl Pts',(-0.182212486373446,0.0302478964060663,
-0.0200000000000001));
#33945=CARTESIAN_POINT('Ctrl Pts',(-0.182939758490654,0.0179487958088136,
-0.0199999999999999));
#33946=CARTESIAN_POINT('Ctrl Pts',(-0.182499636986404,0.00564566013123739,
-0.0199999999999998));
#33947=CARTESIAN_POINT('Ctrl Pts',(-0.180874130922987,-0.0064689356643982,
-0.0199999999999997));
#33948=CARTESIAN_POINT('Ctrl Pts',(-0.179782006632617,-0.0146083358390246,
-0.0199999999999996));
#33949=CARTESIAN_POINT('Ctrl Pts',(-0.178153737391779,-0.0226626229005816,
-0.0200000000000001));
#33950=CARTESIAN_POINT('Ctrl Pts',(-0.175971558313481,-0.0305673708748629,
-0.0200000000000001));
#33951=CARTESIAN_POINT('Ctrl Pts',(-0.17467131893799,-0.0352773713838545,
-0.0200000000000001));
#33952=CARTESIAN_POINT('Ctrl Pts',(-0.173172167501843,-0.0399385102644172,
-0.02));
#33953=CARTESIAN_POINT('Ctrl Pts',(-0.171480129271394,-0.0445086904000026,
-0.02));
#33954=CARTESIAN_POINT('Ctrl Pts',(-0.169172916523709,-0.050740451407697,
-0.02));
#33955=CARTESIAN_POINT('Ctrl Pts',(-0.1665054327452,-0.056812742784086,
-0.0200000000000005));
#33956=CARTESIAN_POINT('Ctrl Pts',(-0.163471173762726,-0.0626921515535454,
-0.0200000000000004));
#33957=CARTESIAN_POINT('Ctrl Pts',(-0.158053708478377,-0.0731894403759654,
-0.0200000000000002));
#33958=CARTESIAN_POINT('Ctrl Pts',(-0.15146825397439,-0.0830745741085914,
-0.0200000000000001));
#33959=CARTESIAN_POINT('Ctrl Pts',(-0.143867977301061,-0.0922205054292428,
-0.0200000000000001));
#33960=CARTESIAN_POINT('Ctrl Pts',(-0.141491856997698,-0.0950798530606812,
-0.02));
#33961=CARTESIAN_POINT('Ctrl Pts',(-0.13901541851784,-0.097867176501796,
-0.0200000000000004));
#33962=CARTESIAN_POINT('Ctrl Pts',(-0.136455144305558,-0.100566063717065,
-0.0200000000000004));
#33963=CARTESIAN_POINT('Ctrl Pts',(-0.129616213094456,-0.107775254015195,
-0.0200000000000004));
#33964=CARTESIAN_POINT('Ctrl Pts',(-0.122162587580282,-0.114377608974371,
-0.0200000000000003));
#33965=CARTESIAN_POINT('Ctrl Pts',(-0.114191093890929,-0.120301882844334,
-0.0200000000000004));
#33966=CARTESIAN_POINT('Ctrl Pts',(-0.109769836460304,-0.123587683584993,
-0.0200000000000004));
#33967=CARTESIAN_POINT('Ctrl Pts',(-0.105188998350819,-0.126664460370265,
-0.0200000000000003));
#33968=CARTESIAN_POINT('Ctrl Pts',(-0.10046396900964,-0.129516366658698,
-0.0200000000000003));
#33969=CARTESIAN_POINT('Ctrl Pts',(-0.0975150341637712,-0.131296267951124,
-0.0200000000000003));
#33970=CARTESIAN_POINT('Ctrl Pts',(-0.0945099247899165,-0.132988524390106,
-0.0200000000000002));
#33971=CARTESIAN_POINT('Ctrl Pts',(-0.0914523710575882,-0.134588691868093,
-0.0200000000000002));
#33972=CARTESIAN_POINT('Ctrl Pts',(-0.0882670061071807,-0.13625574921046,
-0.0200000000000002));
#33973=CARTESIAN_POINT('Ctrl Pts',(-0.0850316946920376,-0.137819083369016,
-0.0199999999999997));
#33974=CARTESIAN_POINT('Ctrl Pts',(-0.0817560776251171,-0.139272781926057,
-0.0199999999999997));
#33975=CARTESIAN_POINT('Ctrl Pts',(-0.0719395593097613,-0.143629291926666,
-0.0199999999999999));
#33976=CARTESIAN_POINT('Ctrl Pts',(-0.0617469188109472,-0.147012280054498,
-0.02));
#33977=CARTESIAN_POINT('Ctrl Pts',(-0.0512986076831915,-0.149302477071082,
-0.02));
#33978=CARTESIAN_POINT('Ctrl Pts',(-0.0449384648191926,-0.150696576082307,
-0.02));
#33979=CARTESIAN_POINT('Ctrl Pts',(-0.0384834618551675,-0.151684836018586,
-0.02));
#33980=CARTESIAN_POINT('Ctrl Pts',(-0.0319621170202007,-0.152230829911641,
-0.02));
#33981=CARTESIAN_POINT('Ctrl Pts',(-0.0685825729128752,0.139614588036674,
-1.58760740822721));
#33982=CARTESIAN_POINT('Ctrl Pts',(-0.115024428893785,0.116801055304812,
-1.58390148054818));
#33983=CARTESIAN_POINT('Ctrl Pts',(-0.182548960740187,0.0215828567384845,
-1.57648962519013));
#33984=CARTESIAN_POINT('Ctrl Pts',(-0.116961678516305,-0.14203802638652,
-1.56537184215306));
#33985=CARTESIAN_POINT('Ctrl Pts',(0.0559048769350007,-0.175112865030439,
-1.55425405911599));
#33986=CARTESIAN_POINT('Ctrl Pts',(0.177489043046939,-0.0480257256248533,
-1.54313627607892));
#33987=CARTESIAN_POINT('Ctrl Pts',(0.136549507894468,0.123166484814191,
-1.53201849304185));
#33988=CARTESIAN_POINT('Ctrl Pts',(-0.0294791068043894,0.181487141263986,
-1.52090071000477));
#33989=CARTESIAN_POINT('Ctrl Pts',(-0.168496105669099,0.0736136087933882,
-1.5097829269677));
#33990=CARTESIAN_POINT('Ctrl Pts',(-0.153191130802483,-0.101700660683814,
-1.49866514393063));
#33991=CARTESIAN_POINT('Ctrl Pts',(0.00242683334840427,-0.183856950102903,
-1.48754736089355));
#33992=CARTESIAN_POINT('Ctrl Pts',(0.155820388725155,-0.0976208199140973,
-1.47642957785648));
#33993=CARTESIAN_POINT('Ctrl Pts',(0.166496760685316,0.078030035232174,
-1.46531179481941));
#33994=CARTESIAN_POINT('Ctrl Pts',(0.0246759993484255,0.182210807009283,
-1.45419401178234));
#33995=CARTESIAN_POINT('Ctrl Pts',(-0.139745612598391,0.119502867680789,
-1.44307622874526));
#33996=CARTESIAN_POINT('Ctrl Pts',(-0.176172414317729,-0.0526597555425937,
-1.43195844570819));
#33997=CARTESIAN_POINT('Ctrl Pts',(-0.0512404048426255,-0.176590393721669,
-1.42084066267112));
#33998=CARTESIAN_POINT('Ctrl Pts',(0.120623364083146,-0.138779552138408,
-1.40972287963405));
#33999=CARTESIAN_POINT('Ctrl Pts',(0.1820065472977,0.0261414484512927,-1.39860509659698));
#34000=CARTESIAN_POINT('Ctrl Pts',(0.0766874125244866,0.167119108331645,
-1.3874873135599));
#34001=CARTESIAN_POINT('Ctrl Pts',(-0.0988707767058873,0.15503008489993,
-1.37636953052283));
#34002=CARTESIAN_POINT('Ctrl Pts',(-0.183871859707572,0.000946859665196946,
-1.36525174748576));
#34003=CARTESIAN_POINT('Ctrl Pts',(-0.100462167484613,-0.154003603442465,
-1.35413396444869));
#34004=CARTESIAN_POINT('Ctrl Pts',(0.0749622096468331,-0.167900042901071,
-1.34301618141161));
#34005=CARTESIAN_POINT('Ctrl Pts',(0.181727664822887,-0.0280145148561602,
-1.33189839837454));
#34006=CARTESIAN_POINT('Ctrl Pts',(0.122046243641521,0.137529893387063,
-1.32078061533747));
#34007=CARTESIAN_POINT('Ctrl Pts',(-0.0494190162937222,0.17710877458793,
-1.3096628323004));
#34008=CARTESIAN_POINT('Ctrl Pts',(-0.175620717250213,0.054471284782664,
-1.29854504926333));
#34009=CARTESIAN_POINT('Ctrl Pts',(-0.140968979581843,-0.118057206406529,
-1.28742726622625));
#34010=CARTESIAN_POINT('Ctrl Pts',(0.0227981919227724,-0.182455473034852,
-1.27630948318918));
#34011=CARTESIAN_POINT('Ctrl Pts',(0.165684184825268,-0.0797402538976839,
-1.26519170015211));
#34012=CARTESIAN_POINT('Ctrl Pts',(0.1568177463056,0.0960101642333705,-1.25407391711503));
#34013=CARTESIAN_POINT('Ctrl Pts',(0.00431976977229057,0.183823547954278,
-1.24295613407796));
#34014=CARTESIAN_POINT('Ctrl Pts',(-0.152134743511917,0.103270407230458,
-1.23183835104089));
#34015=CARTESIAN_POINT('Ctrl Pts',(-0.169246945666504,-0.0718695246646475,
-1.22072056800382));
#34016=CARTESIAN_POINT('Ctrl Pts',(-0.0313435345808448,-0.181183167079792,
-1.20960278496674));
#34017=CARTESIAN_POINT('Ctrl Pts',(0.135267852386276,-0.124548646334775,
-1.19848500192967));
#34018=CARTESIAN_POINT('Ctrl Pts',(0.177985546579018,0.0461616984305375,
-1.1873672188926));
#34019=CARTESIAN_POINT('Ctrl Pts',(0.0576838223577768,0.174591906545624,
-1.17624943585553));
#34020=CARTESIAN_POINT('Ctrl Pts',(-0.115451310830705,0.14311097798737,
-1.16513165281845));
#34021=CARTESIAN_POINT('Ctrl Pts',(-0.182842995135233,-0.0194472703227996,
-1.15401386978138));
#34022=CARTESIAN_POINT('Ctrl Pts',(-0.0827662568575337,-0.164193495360887,
-1.14289608674431));
#34023=CARTESIAN_POINT('Ctrl Pts',(0.0931172382976506,-0.158552632033813,
-1.13177830370724));
#34024=CARTESIAN_POINT('Ctrl Pts',(0.183713369824886,-0.00769122491000194,
-1.12066052067017));
#34025=CARTESIAN_POINT('Ctrl Pts',(0.106043890579969,0.150214681252184,
-1.10954273763309));
#34026=CARTESIAN_POINT('Ctrl Pts',(-0.0687526515134619,0.170536887807008,
-1.09842495459602));
#34027=CARTESIAN_POINT('Ctrl Pts',(-0.180577691259814,0.0346620053128379,
-1.08730717155895));
#34028=CARTESIAN_POINT('Ctrl Pts',(-0.127009131505917,-0.132960286202853,
-1.07618938852188));
#34029=CARTESIAN_POINT('Ctrl Pts',(0.0428888445928814,-0.17880241665738,
-1.06507160548481));
#34030=CARTESIAN_POINT('Ctrl Pts',(0.173504336038483,-0.060876946119833,
-1.05395382244773));
#34031=CARTESIAN_POINT('Ctrl Pts',(0.145204811647398,0.112806559505532,
-1.04283603941066));
#34032=CARTESIAN_POINT('Ctrl Pts',(-0.0160898036409584,0.183168980484762,
-1.03171825637359));
#34033=CARTESIAN_POINT('Ctrl Pts',(-0.162647545726072,0.0857644044013417,
-1.02060047333651));
#34034=CARTESIAN_POINT('Ctrl Pts',(-0.160234156051553,-0.0901929732710832,
-1.00948269029944));
#34035=CARTESIAN_POINT('Ctrl Pts',(-0.0110600915264488,-0.183541362009925,
-0.99836490726237));
#34036=CARTESIAN_POINT('Ctrl Pts',(0.148244063463316,-0.10878168430814,
-0.987247124225296));
#34037=CARTESIAN_POINT('Ctrl Pts',(0.171769434874196,0.0656126393009093,
-0.976129341188226));
#34038=CARTESIAN_POINT('Ctrl Pts',(0.0379688103673882,0.17991144108232,
-0.965011558151151));
#34039=CARTESIAN_POINT('Ctrl Pts',(-0.130607971546202,0.129426871095682,
-0.953893775114081));
#34040=CARTESIAN_POINT('Ctrl Pts',(-0.179559109855943,-0.0396015562923112,
-0.942775992077008));
#34041=CARTESIAN_POINT('Ctrl Pts',(-0.0640495814302482,-0.172358371748057,
-0.931658209039936));
#34042=CARTESIAN_POINT('Ctrl Pts',(0.110123842548254,-0.147249775875683,
-0.920540426002863));
#34043=CARTESIAN_POINT('Ctrl Pts',(0.183433319364821,0.0127269218523267,
-0.909422642965792));
#34044=CARTESIAN_POINT('Ctrl Pts',(0.0887336874904625,0.161046856216992,
-0.898304859928718));
#34045=CARTESIAN_POINT('Ctrl Pts',(-0.0872383533320315,0.16186175243382,
-0.887187076891646));
#34046=CARTESIAN_POINT('Ctrl Pts',(-0.183307582398564,0.0144252358117838,
-0.876069293854574));
#34047=CARTESIAN_POINT('Ctrl Pts',(-0.111482866996807,-0.146223553366767,
-0.864951510817501));
#34048=CARTESIAN_POINT('Ctrl Pts',(0.0624505448146294,-0.172944172048056,
-0.853833727780429));
#34049=CARTESIAN_POINT('Ctrl Pts',(0.179184640777123,-0.0412628368220751,
-0.842715944743356));
#34050=CARTESIAN_POINT('Ctrl Pts',(0.131801051401358,0.128211700099984,
-0.831598161706284));
#34051=CARTESIAN_POINT('Ctrl Pts',(-0.0363009398827759,0.180255371505702,
-0.820480378669211));
#34052=CARTESIAN_POINT('Ctrl Pts',(-0.171154399354551,0.0672006605221613,
-0.80936259563214));
#34053=CARTESIAN_POINT('Ctrl Pts',(-0.149245182428924,-0.107404062841165,
-0.798244812595067));
#34054=CARTESIAN_POINT('Ctrl Pts',(0.00935975675220263,-0.183635922810792,
-0.787127029557995));
#34055=CARTESIAN_POINT('Ctrl Pts',(0.159391965553992,-0.0916731067972864,
-0.776009246520922));
#34056=CARTESIAN_POINT('Ctrl Pts',(0.163434873404623,0.0842543728731427,
-0.76489146348385));
#34057=CARTESIAN_POINT('Ctrl Pts',(0.0177855252092632,0.183012109670541,
-0.753773680446777));
#34058=CARTESIAN_POINT('Ctrl Pts',(-0.144153830975677,0.114146529548942,
-0.742655897409706));
#34059=CARTESIAN_POINT('Ctrl Pts',(-0.174060703964709,-0.0592674322739036,
-0.731538114372633));
#34060=CARTESIAN_POINT('Ctrl Pts',(-0.0445429760552296,-0.17839753495263,
-0.72042033133556));
#34061=CARTESIAN_POINT('Ctrl Pts',(0.125772278341771,-0.134130873380261,
-0.709302548298488));
#34062=CARTESIAN_POINT('Ctrl Pts',(0.180890967276192,0.032988106203831,
-0.698184765261415));
#34063=CARTESIAN_POINT('Ctrl Pts',(0.0703291228835756,0.169892824061108,
-0.687066982224344));
#34064=CARTESIAN_POINT('Ctrl Pts',(-0.104648135740215,0.151190359742707,
-0.675949199187271));
#34065=CARTESIAN_POINT('Ctrl Pts',(-0.183776722635436,-0.00598944157744644,
-0.664831416150198));
#34066=CARTESIAN_POINT('Ctrl Pts',(-0.0945816730450154,-0.157683430699099,
-0.653713633113126));
#34067=CARTESIAN_POINT('Ctrl Pts',(0.081242036168499,-0.164952989521948,
-0.642595850076053));
#34068=CARTESIAN_POINT('Ctrl Pts',(0.182655043268737,-0.0211398287960793,
-0.631478067038982));
#34069=CARTESIAN_POINT('Ctrl Pts',(0.116771775495109,0.142035592865843,
-0.620360284001909));
#34070=CARTESIAN_POINT('Ctrl Pts',(-0.0560643729717556,0.175118654849549,
-0.609242500964836));
#34071=CARTESIAN_POINT('Ctrl Pts',(-0.177550388513388,0.0478081241189917,
-0.598124717927763));
#34072=CARTESIAN_POINT('Ctrl Pts',(-0.136415552918731,-0.123290527271597,
-0.587006934890692));
#34073=CARTESIAN_POINT('Ctrl Pts',(0.0296641702068159,-0.181465683254363,
-0.575889151853619));
#34074=CARTESIAN_POINT('Ctrl Pts',(0.168574070457431,-0.0734339156142763,
-0.564771368816547));
#34075=CARTESIAN_POINT('Ctrl Pts',(0.153084653157532,0.101856988766946,
-0.553653585779474));
#34076=CARTESIAN_POINT('Ctrl Pts',(-0.00261711062509075,0.183855671451842,
-0.542535802742403));
#34077=CARTESIAN_POINT('Ctrl Pts',(-0.15592182666857,0.0974584073406097,
-0.531418019705329));
#34078=CARTESIAN_POINT('Ctrl Pts',(-0.166415589855949,-0.0782023570356304,
-0.520300236668257));
#34079=CARTESIAN_POINT('Ctrl Pts',(-0.0244870176639766,-0.182236503365697,
-0.509182453631186));
#34080=CARTESIAN_POINT('Ctrl Pts',(0.139869551941277,-0.119357721295182,
-0.498064670594112));
#34081=CARTESIAN_POINT('Ctrl Pts',(0.176117668643726,0.0528424449143884,
-0.486946887557041));
#34082=CARTESIAN_POINT('Ctrl Pts',(0.0510571821108666,0.176643486570915,
-0.475829104519967));
#34083=CARTESIAN_POINT('Ctrl Pts',(-0.120767282135644,0.138654321096036,
-0.464711321482895));
#34084=CARTESIAN_POINT('Ctrl Pts',(-0.181979326016571,-0.0263302505796173,
-0.453593538445823));
#34085=CARTESIAN_POINT('Ctrl Pts',(-0.0765139937801866,-0.167198582376871,
-0.44247575540875));
#34086=CARTESIAN_POINT('Ctrl Pts',(0.0990315612963532,-0.154927425139147,
-0.431357972371679));
#34087=CARTESIAN_POINT('Ctrl Pts',(0.183872742689355,-0.000756101129370498,
-0.420240189334605));
#34088=CARTESIAN_POINT('Ctrl Pts',(0.100302341504276,0.154107746339307,
-0.409122406297534));
#34089=CARTESIAN_POINT('Ctrl Pts',(-0.0751363584943781,0.167822182161027,
-0.398004623260461));
#34090=CARTESIAN_POINT('Ctrl Pts',(-0.181756630823041,0.0278259652989701,
-0.386886840223389));
#34091=CARTESIAN_POINT('Ctrl Pts',(-0.121903496635997,-0.13765643719383,
-0.375769057186316));
#34092=CARTESIAN_POINT('Ctrl Pts',(0.0496027324589358,-0.177057409124813,
-0.364651274149244));
#34093=CARTESIAN_POINT('Ctrl Pts',(0.175677134346707,-0.054289056541952,
-0.353533491112171));
#34094=CARTESIAN_POINT('Ctrl Pts',(0.140846424445151,0.118203392142091,
-0.342415708075099));
#34095=CARTESIAN_POINT('Ctrl Pts',(-0.0229874693739835,0.182431722699479,
-0.331297925038026));
#34096=CARTESIAN_POINT('Ctrl Pts',(-0.165766822739796,0.0795683207540087,
-0.320180142000955));
#34097=CARTESIAN_POINT('Ctrl Pts',(-0.156718055506932,-0.0961728042196944,
-0.309062358963882));
#34098=CARTESIAN_POINT('Ctrl Pts',(-0.00412905838771584,-0.183827930642512,
-0.29794457592681));
#34099=CARTESIAN_POINT('Ctrl Pts',(0.152241800199334,-0.103112518319205,
-0.286826792889737));
#34100=CARTESIAN_POINT('Ctrl Pts',(0.169172293136615,0.0720450722777397,
-0.275709009852665));
#34101=CARTESIAN_POINT('Ctrl Pts',(0.031155547779449,0.181215587419735,
-0.264591226815592));
#34102=CARTESIAN_POINT('Ctrl Pts',(-0.135396993113368,0.124408244199608,
-0.25347344377852));
#34103=CARTESIAN_POINT('Ctrl Pts',(-0.17793756067556,-0.0463463249500769,
-0.242355660741447));
#34104=CARTESIAN_POINT('Ctrl Pts',(-0.0575026584572911,-0.174651658969645,
-0.231237877704375));
#34105=CARTESIAN_POINT('Ctrl Pts',(0.115599717800877,-0.142991121590197,
-0.220120094667303));
#34106=CARTESIAN_POINT('Ctrl Pts',(0.182822725577002,0.0196369447459957,
-0.209002311630231));
#34107=CARTESIAN_POINT('Ctrl Pts',(0.0825958599644629,0.164279286494686,
-0.197884528593158));
#34108=CARTESIAN_POINT('Ctrl Pts',(-0.0932816632585158,0.158455916717979,
-0.186766745556086));
#34109=CARTESIAN_POINT('Ctrl Pts',(-0.183721281618962,0.00750067334506049,
-0.175648962519013));
#34110=CARTESIAN_POINT('Ctrl Pts',(-0.105887932579898,-0.150324706413772,
-0.164531179481941));
#34111=CARTESIAN_POINT('Ctrl Pts',(0.0689294256808382,-0.170465296791246,
-0.153413396444868));
#34112=CARTESIAN_POINT('Ctrl Pts',(0.18061377047412,-0.0344749710973018,
-0.142295613407796));
#34113=CARTESIAN_POINT('Ctrl Pts',(0.126870711401792,0.133092601640971,
-0.131177830370724));
#34114=CARTESIAN_POINT('Ctrl Pts',(-0.0430735388430987,0.178756644275882,
-0.120060047333651));
#34115=CARTESIAN_POINT('Ctrl Pts',(-0.173568889044906,0.0606991572905674,
-0.108942264296579));
#34116=CARTESIAN_POINT('Ctrl Pts',(-0.145084867506489,-0.11296141928049,
-0.0978244812595066));
#34117=CARTESIAN_POINT('Ctrl Pts',(0.016274431326597,-0.183144050045734,
-0.0867066982224341));
#34118=CARTESIAN_POINT('Ctrl Pts',(0.162746700955473,-0.0856111115207315,
-0.0755889151853617));
#34119=CARTESIAN_POINT('Ctrl Pts',(0.160120950075793,0.0903886722456795,
-0.0644711321482895));
#34120=CARTESIAN_POINT('Ctrl Pts',(0.0109069706335314,0.18349634534749,
-0.0533533491112173));
#34121=CARTESIAN_POINT('Ctrl Pts',(-0.148428680391759,0.108737123459702,
-0.0422355660741448));
#34122=CARTESIAN_POINT('Ctrl Pts',(-0.171557183147855,-0.066015722996037,
-0.0311177830370724));
#34123=CARTESIAN_POINT('Ctrl Pts',(-0.0826006812134621,-0.141598846131356,
-0.0237059276790242));
#34124=CARTESIAN_POINT('Ctrl Pts',(-0.0319621170202007,-0.152230829911641,
-0.02));
#34125=CARTESIAN_POINT('Ctrl Pts',(-0.0744392439309354,0.151537102412033,
-1.57993827215147));
#34126=CARTESIAN_POINT('Ctrl Pts',(-0.124847044325944,0.126775387360737,
-1.57623234447245));
#34127=CARTESIAN_POINT('Ctrl Pts',(-0.198137894813896,0.0234259443652476,
-1.5688204891144));
#34128=CARTESIAN_POINT('Ctrl Pts',(-0.126949727137059,-0.154167492477815,
-1.55770270607733));
#34129=CARTESIAN_POINT('Ctrl Pts',(0.0606789246064021,-0.1900667869665,
-1.54658492304025));
#34130=CARTESIAN_POINT('Ctrl Pts',(0.192645880859905,-0.0521269260237622,
-1.53546714000318));
#34131=CARTESIAN_POINT('Ctrl Pts',(0.148210276971067,0.133684398496491,
-1.52434935696611));
#34132=CARTESIAN_POINT('Ctrl Pts',(-0.0319965018674015,0.196985400300458,
-1.51323157392904));
#34133=CARTESIAN_POINT('Ctrl Pts',(-0.182884983438119,0.0798999096835992,
-1.50211379089196));
#34134=CARTESIAN_POINT('Ctrl Pts',(-0.166273026361208,-0.11038548084507,
-1.49099600785489));
#34135=CARTESIAN_POINT('Ctrl Pts',(0.00263407498332024,-0.199557581114583,
-1.47987822481782));
#34136=CARTESIAN_POINT('Ctrl Pts',(0.169126812148914,-0.105957238372422,
-1.46876044178075));
#34137=CARTESIAN_POINT('Ctrl Pts',(0.180714902576048,0.0846934808638075,
-1.45764265874367));
#34138=CARTESIAN_POINT('Ctrl Pts',(0.0267832286938344,0.197770864138438,
-1.4465248757066));
#34139=CARTESIAN_POINT('Ctrl Pts',(-0.151679315935036,0.129707923455094,
-1.43540709266953));
#34140=CARTESIAN_POINT('Ctrl Pts',(-0.191216817426186,-0.057156683129376,
-1.42428930963246));
#34141=CARTESIAN_POINT('Ctrl Pts',(-0.0556161256890393,-0.191670490560431,
-1.41317152659538));
#34142=CARTESIAN_POINT('Ctrl Pts',(0.130924105664016,-0.15063075786586,
-1.40205374355831));
#34143=CARTESIAN_POINT('Ctrl Pts',(0.197549161483521,0.0283738211519969,
-1.39093596052124));
#34144=CARTESIAN_POINT('Ctrl Pts',(0.0832362036722443,0.181390396164102,
-1.37981817748417));
#34145=CARTESIAN_POINT('Ctrl Pts',(-0.107313936358152,0.168269019611732,
-1.3687003944471));
#34146=CARTESIAN_POINT('Ctrl Pts',(-0.199573763938466,0.00102771760510595,
-1.35758261141002));
#34147=CARTESIAN_POINT('Ctrl Pts',(-0.109041225395815,-0.167154880839191,
-1.34646482837295));
#34148=CARTESIAN_POINT('Ctrl Pts',(0.0813636755300989,-0.182238019349389,
-1.33534704533588));
#34149=CARTESIAN_POINT('Ctrl Pts',(0.197246463586825,-0.0304068397613748,
-1.32422926229881));
#34150=CARTESIAN_POINT('Ctrl Pts',(0.132468493312827,0.149274383372008,
-1.31311147926173));
#34151=CARTESIAN_POINT('Ctrl Pts',(-0.0536391980130076,0.192233139030937,
-1.30199369622466));
#34152=CARTESIAN_POINT('Ctrl Pts',(-0.190618007687202,0.0591229095519548,
-1.29087591318759));
#34153=CARTESIAN_POINT('Ctrl Pts',(-0.153007153451631,-0.128138808625108,
-1.27975813015052));
#34154=CARTESIAN_POINT('Ctrl Pts',(0.0247450641999012,-0.198036423641172,
-1.26864034711344));
#34155=CARTESIAN_POINT('Ctrl Pts',(0.179832936063426,-0.0865497452034227,
-1.25752256407637));
#34156=CARTESIAN_POINT('Ctrl Pts',(0.170209339984542,0.104209039288979,
-1.2464047810393));
#34157=CARTESIAN_POINT('Ctrl Pts',(0.00468866043001303,0.199521326559181,
-1.23528699800223));
#34158=CARTESIAN_POINT('Ctrl Pts',(-0.165126427919824,0.11208927732182,
-1.22416921496515));
#34159=CARTESIAN_POINT('Ctrl Pts',(-0.183699942098113,-0.0780068879088045,
-1.21305143192808));
#34160=CARTESIAN_POINT('Ctrl Pts',(-0.0340201441448589,-0.196655467965102,
-1.20193364889101));
#34161=CARTESIAN_POINT('Ctrl Pts',(0.146819173328295,-0.135184590953742,
-1.19081586585394));
#34162=CARTESIAN_POINT('Ctrl Pts',(0.193184783761432,0.0501037185365196,
-1.17969808281687));
#34163=CARTESIAN_POINT('Ctrl Pts',(0.0626097846870554,0.189501340759367,
-1.16858029977979));
#34164=CARTESIAN_POINT('Ctrl Pts',(-0.125310380233048,0.155332069753783,
-1.15746251674272));
#34165=CARTESIAN_POINT('Ctrl Pts',(-0.198457038542795,-0.0211079876106242,
-1.14634473370565));
#34166=CARTESIAN_POINT('Ctrl Pts',(-0.0898341564306036,-0.178214947820184,
-1.13522695066857));
#34167=CARTESIAN_POINT('Ctrl Pts',(0.101069069319104,-0.172092377853052,
-1.1241091676315));
#34168=CARTESIAN_POINT('Ctrl Pts',(0.199401739668498,-0.0083480240371076,
-1.11299138459443));
#34169=CARTESIAN_POINT('Ctrl Pts',(0.115099604797503,0.163042400201931,
-1.10187360155736));
#34170=CARTESIAN_POINT('Ctrl Pts',(-0.0746238465478801,0.185100040017679,
-1.09075581852028));
#34171=CARTESIAN_POINT('Ctrl Pts',(-0.195998286988311,0.0376219986948521,
-1.07963803548322));
#34172=CARTESIAN_POINT('Ctrl Pts',(-0.137855191487726,-0.144314550437683,
-1.06852025244614));
#34173=CARTESIAN_POINT('Ctrl Pts',(0.0465513763769294,-0.194071411201035,
-1.05740246940907));
#34174=CARTESIAN_POINT('Ctrl Pts',(0.188320896182345,-0.0660755881489248,
-1.046284686372));
#34175=CARTESIAN_POINT('Ctrl Pts',(0.15760470823831,0.122439777969681,-1.03516690333492));
#34176=CARTESIAN_POINT('Ctrl Pts',(-0.0174638070162759,0.198810861706915,
-1.02404912029785));
#34177=CARTESIAN_POINT('Ctrl Pts',(-0.176536980414133,0.0930883335032248,
-1.01293133726078));
#34178=CARTESIAN_POINT('Ctrl Pts',(-0.173917497139423,-0.0978950840282937,
-1.00181355422371));
#34179=CARTESIAN_POINT('Ctrl Pts',(-0.0120045780738169,-0.199215043090168,
-0.990695771186635));
#34180=CARTESIAN_POINT('Ctrl Pts',(0.160903499719639,-0.118071194904261,
-0.979577988149561));
#34181=CARTESIAN_POINT('Ctrl Pts',(0.186437841559585,0.0712156901444556,
-0.96846020511249));
#34182=CARTESIAN_POINT('Ctrl Pts',(0.0412111913662969,0.195275141772624,
-0.957342422075417));
#34183=CARTESIAN_POINT('Ctrl Pts',(-0.141761357737385,0.140479396142641,
-0.946224639038345));
#34184=CARTESIAN_POINT('Ctrl Pts',(-0.194892722901607,-0.0429833671103725,
-0.935106856001272));
#34185=CARTESIAN_POINT('Ctrl Pts',(-0.0695191535292426,-0.187077071231953,
-0.9239890729642));
#34186=CARTESIAN_POINT('Ctrl Pts',(0.119527967964621,-0.159824304041645,
-0.912871289927129));
#34187=CARTESIAN_POINT('Ctrl Pts',(0.199097774045392,0.0138137488871811,
-0.901753506890054));
#34188=CARTESIAN_POINT('Ctrl Pts',(0.0963111812148712,0.174799598572606,
-0.890635723852983));
#34189=CARTESIAN_POINT('Ctrl Pts',(-0.0946881516397165,0.175684083590979,
-0.87951794081591));
#34190=CARTESIAN_POINT('Ctrl Pts',(-0.198961299656857,0.0156570919075729,
-0.868400157778838));
#34191=CARTESIAN_POINT('Ctrl Pts',(-0.121003047538591,-0.158710446330799,
-0.857282374741765));
#34192=CARTESIAN_POINT('Ctrl Pts',(0.0677835657315107,-0.18771289647989,
-0.846164591704693));
#34193=CARTESIAN_POINT('Ctrl Pts',(0.194486275696159,-0.0447865141977529,
-0.835046808667621));
#34194=CARTESIAN_POINT('Ctrl Pts',(0.143056321728893,0.139160454517608,
-0.823929025630549));
#34195=CARTESIAN_POINT('Ctrl Pts',(-0.0394008915688968,0.195648442446455,
-0.812811242593476));
#34196=CARTESIAN_POINT('Ctrl Pts',(-0.185770284523904,0.0729393218782279,
-0.801693459556404));
#34197=CARTESIAN_POINT('Ctrl Pts',(-0.161990110147327,-0.116575930202614,
-0.790575676519331));
#34198=CARTESIAN_POINT('Ctrl Pts',(0.0101590416693245,-0.199317678996392,
-0.779457893482259));
#34199=CARTESIAN_POINT('Ctrl Pts',(0.173003387020459,-0.0995016148994445,
-0.768340110445186));
#34200=CARTESIAN_POINT('Ctrl Pts',(0.177391542653899,0.0914493514630801,
-0.757222327408114));
#34201=CARTESIAN_POINT('Ctrl Pts',(0.0193043362659213,0.198640594767233,
-0.746104544371042));
#34202=CARTESIAN_POINT('Ctrl Pts',(-0.15646397811889,0.123894175970298,
-0.73498676133397));
#34203=CARTESIAN_POINT('Ctrl Pts',(-0.188924775652256,-0.0643286284082972,
-0.723868978296897));
#34204=CARTESIAN_POINT('Ctrl Pts',(-0.0483467638957979,-0.193631954255882,
-0.712751195259825));
#34205=CARTESIAN_POINT('Ctrl Pts',(0.136512716125805,-0.145585100968826,
-0.701633412222752));
#34206=CARTESIAN_POINT('Ctrl Pts',(0.19633831549425,0.0358051554532093,
-0.690515629185681));
#34207=CARTESIAN_POINT('Ctrl Pts',(0.0763349421205001,0.184400975864033,
-0.679397846148607));
#34208=CARTESIAN_POINT('Ctrl Pts',(-0.113584658207261,0.164101397642091,
-0.668280063111536));
#34209=CARTESIAN_POINT('Ctrl Pts',(-0.199470502549766,-0.00650091537335537,
-0.657162280074462));
#34210=CARTESIAN_POINT('Ctrl Pts',(-0.102658560799958,-0.171148950281995,
-0.646044497037391));
#34211=CARTESIAN_POINT('Ctrl Pts',(0.0881797735333642,-0.179039299673989,
-0.634926714000318));
#34212=CARTESIAN_POINT('Ctrl Pts',(0.198253036356188,-0.0229450836498757,
-0.623808930963246));
#34213=CARTESIAN_POINT('Ctrl Pts',(0.126743607175127,0.154164851144433,
-0.612691147926174));
#34214=CARTESIAN_POINT('Ctrl Pts',(-0.0608520409518781,0.190073071212465,
-0.601573364889101));
#34215=CARTESIAN_POINT('Ctrl Pts',(-0.192712464978101,0.0518907422399437,
-0.590455581852028));
#34216=CARTESIAN_POINT('Ctrl Pts',(-0.14806488278868,-0.133819033672054,
-0.579337798814956));
#34217=CARTESIAN_POINT('Ctrl Pts',(0.0321973689269302,-0.196962109864641,
-0.568220015777883));
#34218=CARTESIAN_POINT('Ctrl Pts',(0.182969606100265,-0.0797048714424761,
-0.557102232740812));
#34219=CARTESIAN_POINT('Ctrl Pts',(0.166157455961192,0.11055515870665,-0.545984449703739));
#34220=CARTESIAN_POINT('Ctrl Pts',(-0.00284060116063022,0.199556193271956,
-0.534866666666666));
#34221=CARTESIAN_POINT('Ctrl Pts',(-0.169236912477511,0.105780956429914,
-0.523748883629594));
#34222=CARTESIAN_POINT('Ctrl Pts',(-0.180626800090086,-0.0848805182439657,
-0.512631100592522));
#34223=CARTESIAN_POINT('Ctrl Pts',(-0.0265781087470362,-0.197798754858514,
-0.501513317555449));
#34224=CARTESIAN_POINT('Ctrl Pts',(0.151813839190521,-0.129550382162242,
-0.490395534518377));
#34225=CARTESIAN_POINT('Ctrl Pts',(0.191157396695698,0.0573549734257742,
-0.479277751481304));
#34226=CARTESIAN_POINT('Ctrl Pts',(0.0554172564859194,0.191728117321693,
-0.468159968444232));
#34227=CARTESIAN_POINT('Ctrl Pts',(-0.13108031372914,0.150494832605041,
-0.457042185407159));
#34228=CARTESIAN_POINT('Ctrl Pts',(-0.1975196156164,-0.0285787462093131,
-0.445924402370088));
#34229=CARTESIAN_POINT('Ctrl Pts',(-0.0830479756769845,-0.181476656967502,
-0.434806619333015));
#34230=CARTESIAN_POINT('Ctrl Pts',(0.107488451294552,-0.168157593127565,
-0.423688836295943));
#34231=CARTESIAN_POINT('Ctrl Pts',(0.199574722323279,-0.000820669071094855,
-0.41257105325887));
#34232=CARTESIAN_POINT('Ctrl Pts',(0.108867750930925,0.167267917113166,
-0.401453270221799));
#34233=CARTESIAN_POINT('Ctrl Pts',(-0.0815526959764324,0.18215350962083,
-0.390335487184724));
#34234=CARTESIAN_POINT('Ctrl Pts',(-0.197277903164835,0.0302021888437342,
-0.379217704147654));
#34235=CARTESIAN_POINT('Ctrl Pts',(-0.132313556297296,-0.149411733501928,
-0.368099921110581));
#34236=CARTESIAN_POINT('Ctrl Pts',(0.0538386027867795,-0.192177387167509,
-0.356982138073509));
#34237=CARTESIAN_POINT('Ctrl Pts',(0.190679242572821,-0.0589251197653465,
-0.345864355036436));
#34238=CARTESIAN_POINT('Ctrl Pts',(0.152874132607884,0.128297478024148,
-0.334746571999364));
#34239=CARTESIAN_POINT('Ctrl Pts',(-0.0249505051707323,0.198010645124367,
-0.323628788962291));
#34240=CARTESIAN_POINT('Ctrl Pts',(-0.179922630917619,0.0863631296730007,
-0.312511005925219));
#34241=CARTESIAN_POINT('Ctrl Pts',(-0.170101135999703,-0.104385568064449,
-0.301393222888146));
#34242=CARTESIAN_POINT('Ctrl Pts',(-0.00448166307377801,-0.199526083511052,
-0.290275439851074));
#34243=CARTESIAN_POINT('Ctrl Pts',(0.165242626810163,-0.111917905343786,
-0.279157656814001));
#34244=CARTESIAN_POINT('Ctrl Pts',(0.183618914547724,0.0781974265695377,
-0.26803987377693));
#34245=CARTESIAN_POINT('Ctrl Pts',(0.0338161040400543,0.196690656869379,
-0.256922090739857));
#34246=CARTESIAN_POINT('Ctrl Pts',(-0.146959342144907,0.135032199050898,
-0.245804307702785));
#34247=CARTESIAN_POINT('Ctrl Pts',(-0.193132700058226,-0.0503041114051506,
-0.234686524665712));
#34248=CARTESIAN_POINT('Ctrl Pts',(-0.0624131501309722,-0.189566195795832,
-0.22356874162864));
#34249=CARTESIAN_POINT('Ctrl Pts',(0.125471460551042,-0.155201978110864,
-0.212450958591567));
#34250=CARTESIAN_POINT('Ctrl Pts',(0.198435038047255,0.0213138594532229,
-0.201333175554495));
#34251=CARTESIAN_POINT('Ctrl Pts',(0.0896492083402993,0.178308065165666,
-0.190215392517423));
#34252=CARTESIAN_POINT('Ctrl Pts',(-0.101247535498635,0.171987403445101,
-0.17909760948035));
#34253=CARTESIAN_POINT('Ctrl Pts',(-0.199410327097406,0.0081412001484483,
-0.167979826443278));
#34254=CARTESIAN_POINT('Ctrl Pts',(-0.114930328622562,-0.163161821061985,
-0.156862043406206));
#34255=CARTESIAN_POINT('Ctrl Pts',(0.0748157165056128,-0.185022335422193,
-0.145744260369133));
#34256=CARTESIAN_POINT('Ctrl Pts',(0.196037447219847,-0.0374189925228408,
-0.134626477332061));
#34257=CARTESIAN_POINT('Ctrl Pts',(0.137704950873262,0.144458165072649,
-0.123508694294988));
#34258=CARTESIAN_POINT('Ctrl Pts',(-0.0467518427601612,0.194021730045504,
-0.112390911257916));
#34259=CARTESIAN_POINT('Ctrl Pts',(-0.188390961751301,0.0658826168813301,
-0.101273128220844));
#34260=CARTESIAN_POINT('Ctrl Pts',(-0.157474521358699,-0.122607862135579,
-0.090155345183771));
#34261=CARTESIAN_POINT('Ctrl Pts',(0.0176642011505863,-0.198783802310435,
-0.0790375621466987));
#34262=CARTESIAN_POINT('Ctrl Pts',(0.176644603094283,-0.0929219500380387,
-0.0679197791096262));
#34263=CARTESIAN_POINT('Ctrl Pts',(0.173794623836686,0.0981074948943239,
-0.056801996072554));
#34264=CARTESIAN_POINT('Ctrl Pts',(0.0118383812833686,0.199166182189015,
-0.0456842130354818));
#34265=CARTESIAN_POINT('Ctrl Pts',(-0.161103882178133,0.118022828741753,
-0.0345664299984093));
#34266=CARTESIAN_POINT('Ctrl Pts',(-0.186207464404562,-0.0716531955373244,
-0.0234486469613369));
#34267=CARTESIAN_POINT('Ctrl Pts',(-0.0896544413042297,-0.153690808026425,
-0.0160367916032887));
#34268=CARTESIAN_POINT('Ctrl Pts',(-0.0346915509926754,-0.165230719704803,
-0.0123308639242645));
#34269=CARTESIAN_POINT('Ctrl Pts',(-0.0802959149489957,0.163459616787393,
-1.57226913607574));
#34270=CARTESIAN_POINT('Ctrl Pts',(-0.134669659758104,0.136749719416661,
-1.56856320839671));
#34271=CARTESIAN_POINT('Ctrl Pts',(-0.213726828887605,0.0252690319920107,
-1.56115135303866));
#34272=CARTESIAN_POINT('Ctrl Pts',(-0.136937775757814,-0.166296958569109,
-1.55003357000159));
#34273=CARTESIAN_POINT('Ctrl Pts',(0.0654529722778036,-0.205020708902561,
-1.53891578696452));
#34274=CARTESIAN_POINT('Ctrl Pts',(0.20780271867287,-0.0562281264226708,
-1.52779800392744));
#34275=CARTESIAN_POINT('Ctrl Pts',(0.159871046047665,0.14420231217879,-1.51668022089037));
#34276=CARTESIAN_POINT('Ctrl Pts',(-0.0345138969304135,0.212483659336931,
-1.5055624378533));
#34277=CARTESIAN_POINT('Ctrl Pts',(-0.19727386120714,0.0861862105738098,
-1.49444465481623));
#34278=CARTESIAN_POINT('Ctrl Pts',(-0.179354921919933,-0.119070301006325,
-1.48332687177916));
#34279=CARTESIAN_POINT('Ctrl Pts',(0.00284131661823614,-0.215258212126264,
-1.47220908874208));
#34280=CARTESIAN_POINT('Ctrl Pts',(0.182433235572673,-0.114293656830746,
-1.46109130570501));
#34281=CARTESIAN_POINT('Ctrl Pts',(0.19493304446678,0.0913569264954411,
-1.44997352266794));
#34282=CARTESIAN_POINT('Ctrl Pts',(0.0288904580392435,0.213330921267592,
-1.43885573963087));
#34283=CARTESIAN_POINT('Ctrl Pts',(-0.163613019271682,0.1399129792294,-1.42773795659379));
#34284=CARTESIAN_POINT('Ctrl Pts',(-0.206261220534644,-0.0616536107161584,
-1.41662017355672));
#34285=CARTESIAN_POINT('Ctrl Pts',(-0.0599918465354529,-0.206750587399193,
-1.40550239051965));
#34286=CARTESIAN_POINT('Ctrl Pts',(0.141224847244886,-0.162481963593313,
-1.39438460748258));
#34287=CARTESIAN_POINT('Ctrl Pts',(0.213091775669342,0.0306061938527011,
-1.38326682444551));
#34288=CARTESIAN_POINT('Ctrl Pts',(0.0897849948200019,0.195661683996559,
-1.37214904140843));
#34289=CARTESIAN_POINT('Ctrl Pts',(-0.115757096010416,0.181507954323534,
-1.36103125837136));
#34290=CARTESIAN_POINT('Ctrl Pts',(-0.215275668169361,0.00110857554501473,
-1.34991347533429));
#34291=CARTESIAN_POINT('Ctrl Pts',(-0.117620283307016,-0.180306158235917,
-1.33879569229721));
#34292=CARTESIAN_POINT('Ctrl Pts',(0.0877651414133644,-0.196575995797707,
-1.32767790926014));
#34293=CARTESIAN_POINT('Ctrl Pts',(0.212765262350764,-0.0327991646665892,
-1.31656012622307));
#34294=CARTESIAN_POINT('Ctrl Pts',(0.142890742984133,0.161018873356952,
-1.305442343186));
#34295=CARTESIAN_POINT('Ctrl Pts',(-0.0578593797322928,0.207357503473944,
-1.29432456014893));
#34296=CARTESIAN_POINT('Ctrl Pts',(-0.205615298124191,0.0637745343212453,
-1.28320677711185));
#34297=CARTESIAN_POINT('Ctrl Pts',(-0.165045327321419,-0.138220410843686,
-1.27208899407478));
#34298=CARTESIAN_POINT('Ctrl Pts',(0.0266919364770298,-0.213617374247491,
-1.26097121103771));
#34299=CARTESIAN_POINT('Ctrl Pts',(0.193981687301585,-0.0933592365091615,
-1.24985342800064));
#34300=CARTESIAN_POINT('Ctrl Pts',(0.183600933663484,0.112407914344587,
-1.23873564496356));
#34301=CARTESIAN_POINT('Ctrl Pts',(0.00505755108773542,0.215219105164084,
-1.22761786192649));
#34302=CARTESIAN_POINT('Ctrl Pts',(-0.178118112327731,0.120908147413182,
-1.21650007888942));
#34303=CARTESIAN_POINT('Ctrl Pts',(-0.198152938529722,-0.0841442511529614,
-1.20538229585235));
#34304=CARTESIAN_POINT('Ctrl Pts',(-0.0366967537088725,-0.212127768850411,
-1.19426451281527));
#34305=CARTESIAN_POINT('Ctrl Pts',(0.158370494270313,-0.145820535572709,
-1.1831467297782));
#34306=CARTESIAN_POINT('Ctrl Pts',(0.208384020943847,0.0540457386425016,
-1.17202894674113));
#34307=CARTESIAN_POINT('Ctrl Pts',(0.0675357470163338,0.20441077497311,
-1.16091116370406));
#34308=CARTESIAN_POINT('Ctrl Pts',(-0.135169449635391,0.167553161520197,
-1.14979338066698));
#34309=CARTESIAN_POINT('Ctrl Pts',(-0.214071081950358,-0.0227687048984483,
-1.13867559762991));
#34310=CARTESIAN_POINT('Ctrl Pts',(-0.0969020560036732,-0.192236400279482,
-1.12755781459284));
#34311=CARTESIAN_POINT('Ctrl Pts',(0.109020900340556,-0.185632123672291,
-1.11644003155577));
#34312=CARTESIAN_POINT('Ctrl Pts',(0.215090109512111,-0.00900482316421355,
-1.1053222485187));
#34313=CARTESIAN_POINT('Ctrl Pts',(0.124155319015036,0.175870119151678,
-1.09420446548162));
#34314=CARTESIAN_POINT('Ctrl Pts',(-0.0804950415822979,0.199663192228349,
-1.08308668244455));
#34315=CARTESIAN_POINT('Ctrl Pts',(-0.211418882716809,0.0405819920768663,
-1.07196889940748));
#34316=CARTESIAN_POINT('Ctrl Pts',(-0.148701251469534,-0.155668814672513,
-1.06085111637041));
#34317=CARTESIAN_POINT('Ctrl Pts',(0.0502139081609773,-0.209340405744691,
-1.04973333333333));
#34318=CARTESIAN_POINT('Ctrl Pts',(0.203137456326208,-0.0712742301780164,
-1.03861555029626));
#34319=CARTESIAN_POINT('Ctrl Pts',(0.170004604829223,0.13207299643383,-1.02749776725919));
#34320=CARTESIAN_POINT('Ctrl Pts',(-0.0188378103915933,0.214452742929068,
-1.01637998422212));
#34321=CARTESIAN_POINT('Ctrl Pts',(-0.190426415102195,0.100412262605108,
-1.00526220118504));
#34322=CARTESIAN_POINT('Ctrl Pts',(-0.187600838227293,-0.105597194785504,
-0.994144418147971));
#34323=CARTESIAN_POINT('Ctrl Pts',(-0.0129490646211849,-0.214888724170412,
-0.9830266351109));
#34324=CARTESIAN_POINT('Ctrl Pts',(0.173562935975961,-0.127360705500382,
-0.971908852073825));
#34325=CARTESIAN_POINT('Ctrl Pts',(0.201106248244974,0.0768187409880018,
-0.960791069036756));
#34326=CARTESIAN_POINT('Ctrl Pts',(0.0444535723652056,0.210638842462928,
-0.94967328599968));
#34327=CARTESIAN_POINT('Ctrl Pts',(-0.152914743928569,0.151531921189599,
-0.93855550296261));
#34328=CARTESIAN_POINT('Ctrl Pts',(-0.210226335947272,-0.0463651779284336,
-0.927437719925536));
#34329=CARTESIAN_POINT('Ctrl Pts',(-0.0749887256282371,-0.201795770715849,
-0.916319936888466));
#34330=CARTESIAN_POINT('Ctrl Pts',(0.128932093380988,-0.172398832207608,
-0.905202153851391));
#34331=CARTESIAN_POINT('Ctrl Pts',(0.214762228725962,0.0149005759220357,
-0.894084370814321));
#34332=CARTESIAN_POINT('Ctrl Pts',(0.10388867493928,0.188552340928219,-0.882966587777247));
#34333=CARTESIAN_POINT('Ctrl Pts',(-0.102137949947401,0.189506414748137,
-0.871848804740174));
#34334=CARTESIAN_POINT('Ctrl Pts',(-0.214615016915151,0.016888948003362,
-0.860731021703104));
#34335=CARTESIAN_POINT('Ctrl Pts',(-0.130523228080374,-0.171197339294831,
-0.849613238666029));
#34336=CARTESIAN_POINT('Ctrl Pts',(0.0731165866483921,-0.202481620911723,
-0.838495455628959));
#34337=CARTESIAN_POINT('Ctrl Pts',(0.209787910615195,-0.0483101915734308,
-0.827377672591884));
#34338=CARTESIAN_POINT('Ctrl Pts',(0.154311592056428,0.150109208935231,
-0.816259889554814));
#34339=CARTESIAN_POINT('Ctrl Pts',(-0.0425008432550175,0.211041513387208,
-0.80514210651774));
#34340=CARTESIAN_POINT('Ctrl Pts',(-0.200386169693257,0.0786779832342944,
-0.794024323480669));
#34341=CARTESIAN_POINT('Ctrl Pts',(-0.17473503786573,-0.125747797564063,
-0.782906540443596));
#34342=CARTESIAN_POINT('Ctrl Pts',(0.0109583265864464,-0.214999435181992,
-0.771788757406523));
#34343=CARTESIAN_POINT('Ctrl Pts',(0.186614808486925,-0.107330123001603,
-0.760670974369452));
#34344=CARTESIAN_POINT('Ctrl Pts',(0.191348211903174,0.098644330053018,
-0.749553191332378));
#34345=CARTESIAN_POINT('Ctrl Pts',(0.0208231473225793,0.214269079863924,
-0.738435408295307));
#34346=CARTESIAN_POINT('Ctrl Pts',(-0.168774125262104,0.133641822391654,
-0.727317625258233));
#34347=CARTESIAN_POINT('Ctrl Pts',(-0.203788847339803,-0.0693898245426907,
-0.716199842221162));
#34348=CARTESIAN_POINT('Ctrl Pts',(-0.0521505517363663,-0.208866373559133,
-0.705082059184089));
#34349=CARTESIAN_POINT('Ctrl Pts',(0.147253153909839,-0.157039328557391,
-0.693964276147018));
#34350=CARTESIAN_POINT('Ctrl Pts',(0.211785663712306,0.0386222047025875,
-0.682846493109943));
#34351=CARTESIAN_POINT('Ctrl Pts',(0.0823407613574247,0.198909127666958,
-0.671728710072873));
#34352=CARTESIAN_POINT('Ctrl Pts',(-0.122521180674308,0.177012435541474,
-0.660610927035799));
#34353=CARTESIAN_POINT('Ctrl Pts',(-0.215164282464097,-0.00701238916926441,
-0.649493143998728));
#34354=CARTESIAN_POINT('Ctrl Pts',(-0.110735448554901,-0.184614469864892,
-0.638375360961654));
#34355=CARTESIAN_POINT('Ctrl Pts',(0.0951175108982293,-0.193125609826029,
-0.627257577924583));
#34356=CARTESIAN_POINT('Ctrl Pts',(0.21385102944364,-0.0247503385036721,
-0.61613979488751));
#34357=CARTESIAN_POINT('Ctrl Pts',(0.136715438855145,0.166294109423022,
-0.605022011850438));
#34358=CARTESIAN_POINT('Ctrl Pts',(-0.0656397089320004,0.205027487575381,
-0.593904228813365));
#34359=CARTESIAN_POINT('Ctrl Pts',(-0.207874541442814,0.0559733603608955,
-0.582786445776292));
#34360=CARTESIAN_POINT('Ctrl Pts',(-0.159714212658629,-0.14434754007251,
-0.571668662739221));
#34361=CARTESIAN_POINT('Ctrl Pts',(0.0347305676470442,-0.212458536474919,
-0.560550879702147));
#34362=CARTESIAN_POINT('Ctrl Pts',(0.197365141743099,-0.0859758272706753,
-0.549433096665076));
#34363=CARTESIAN_POINT('Ctrl Pts',(0.179230258764851,0.119253328646353,
-0.538315313628003));
#34364=CARTESIAN_POINT('Ctrl Pts',(-0.00306409169616951,0.215256715092069,
-0.527197530590932));
#34365=CARTESIAN_POINT('Ctrl Pts',(-0.182551998286452,0.114103505519217,
-0.516079747553858));
#34366=CARTESIAN_POINT('Ctrl Pts',(-0.194838010324222,-0.0915586794523007,
-0.504961964516786));
#34367=CARTESIAN_POINT('Ctrl Pts',(-0.0286691998300962,-0.213361006351331,
-0.493844181479714));
#34368=CARTESIAN_POINT('Ctrl Pts',(0.163758126439765,-0.139743043029301,
-0.482726398442641));
#34369=CARTESIAN_POINT('Ctrl Pts',(0.20619712474767,0.0618675019371596,
-0.471608615405569));
#34370=CARTESIAN_POINT('Ctrl Pts',(0.0597773308609723,0.206812748072472,
-0.460490832368497));
#34371=CARTESIAN_POINT('Ctrl Pts',(-0.141393345322637,0.162335344114046,
-0.449373049331423));
#34372=CARTESIAN_POINT('Ctrl Pts',(-0.21305990521623,-0.0308272418390084,
-0.438255266294353));
#34373=CARTESIAN_POINT('Ctrl Pts',(-0.0895819575737826,-0.195754731558133,
-0.427137483257279));
#34374=CARTESIAN_POINT('Ctrl Pts',(0.11594534129275,-0.181387761115983,
-0.416019700220208));
#34375=CARTESIAN_POINT('Ctrl Pts',(0.215276701957203,-0.000885237012819617,
-0.404901917183134));
#34376=CARTESIAN_POINT('Ctrl Pts',(0.117433160357574,0.180428087887024,
-0.393784134146063));
#34377=CARTESIAN_POINT('Ctrl Pts',(-0.087969033458487,0.196484837080633,
-0.382666351108989));
#34378=CARTESIAN_POINT('Ctrl Pts',(-0.212799175506629,0.0325784123884988,
-0.371548568071918));
#34379=CARTESIAN_POINT('Ctrl Pts',(-0.142723615958594,-0.161167029810026,
-0.360430785034845));
#34380=CARTESIAN_POINT('Ctrl Pts',(0.0580744731146232,-0.207297365210204,
-0.349313001997773));
#34381=CARTESIAN_POINT('Ctrl Pts',(0.205681350798936,-0.0635611829887412,
-0.3381952189607));
#34382=CARTESIAN_POINT('Ctrl Pts',(0.164901840770617,0.138391563906206,
-0.327077435923628));
#34383=CARTESIAN_POINT('Ctrl Pts',(-0.0269135409674812,0.213589567549256,
-0.315959652886555));
#34384=CARTESIAN_POINT('Ctrl Pts',(-0.194078439095441,0.0931579385919925,
-0.304841869849484));
#34385=CARTESIAN_POINT('Ctrl Pts',(-0.183484216492474,-0.112598331909203,
-0.293724086812411));
#34386=CARTESIAN_POINT('Ctrl Pts',(-0.0048342677598399,-0.215224236379592,
-0.282606303775339));
#34387=CARTESIAN_POINT('Ctrl Pts',(0.178243453420992,-0.120723292368367,
-0.271488520738266));
#34388=CARTESIAN_POINT('Ctrl Pts',(0.198065535958834,0.0843497808613357,
-0.260370737701194));
#34389=CARTESIAN_POINT('Ctrl Pts',(0.0364766603006594,0.212165726319023,
-0.249252954664121));
#34390=CARTESIAN_POINT('Ctrl Pts',(-0.158521691176445,0.145656153902189,
-0.238135171627049));
#34391=CARTESIAN_POINT('Ctrl Pts',(-0.208327839440892,-0.0542618978602245,
-0.227017388589977));
#34392=CARTESIAN_POINT('Ctrl Pts',(-0.0673236418046539,-0.204480732622019,
-0.215899605552904));
#34393=CARTESIAN_POINT('Ctrl Pts',(0.135343203301208,-0.167412834631532,
-0.204781822515832));
#34394=CARTESIAN_POINT('Ctrl Pts',(0.214047350517508,0.02299077416045,-0.19366403947876));
#34395=CARTESIAN_POINT('Ctrl Pts',(0.096702556716136,0.192336843836647,
-0.182546256441687));
#34396=CARTESIAN_POINT('Ctrl Pts',(-0.109213407738754,0.185518890172223,
-0.171428473404615));
#34397=CARTESIAN_POINT('Ctrl Pts',(-0.215099372575849,0.0087817269518365,
-0.160310690367542));
#34398=CARTESIAN_POINT('Ctrl Pts',(-0.123972724665226,-0.175998935710198,
-0.14919290733047));
#34399=CARTESIAN_POINT('Ctrl Pts',(0.0807020073303874,-0.19957937405314,
-0.138075124293397));
#34400=CARTESIAN_POINT('Ctrl Pts',(0.211461123965574,-0.0403630139483802,
-0.126957341256325));
#34401=CARTESIAN_POINT('Ctrl Pts',(0.148539190344733,0.155823728504327,
-0.115839558219253));
#34402=CARTESIAN_POINT('Ctrl Pts',(-0.0504301466772234,0.209286815815126,
-0.10472177518218));
#34403=CARTESIAN_POINT('Ctrl Pts',(-0.203213034457697,0.0710660764720931,
-0.0936039921451079));
#34404=CARTESIAN_POINT('Ctrl Pts',(-0.169864175210909,-0.132254304990668,
-0.0824862091080356));
#34405=CARTESIAN_POINT('Ctrl Pts',(0.0190539709745751,-0.214423554575135,
-0.0713684260709631));
#34406=CARTESIAN_POINT('Ctrl Pts',(0.190542505233092,-0.100232788555346,
-0.0602506430338908));
#34407=CARTESIAN_POINT('Ctrl Pts',(0.187468297597579,0.105826317542969,
-0.0491328599968185));
#34408=CARTESIAN_POINT('Ctrl Pts',(0.012769791933206,0.21483601903054,-0.0380150769597463));
#34409=CARTESIAN_POINT('Ctrl Pts',(-0.173779083964507,0.127308534023805,
-0.0268972939226738));
#34410=CARTESIAN_POINT('Ctrl Pts',(-0.200857745661268,-0.0772906680786118,
-0.0157795108856014));
#34411=CARTESIAN_POINT('Ctrl Pts',(-0.0967082013949975,-0.165782769921495,
-0.00836765552755316));
#34412=CARTESIAN_POINT('Ctrl Pts',(-0.03742098496515,-0.178230609497964,
-0.00466172784852903));
#34413=CARTESIAN_POINT('Ctrl Pts',(-0.0861525859670559,0.175382131162753,
-1.5646));
#34414=CARTESIAN_POINT('Ctrl Pts',(-0.144492275190263,0.146724051472585,
-1.56089407232098));
#34415=CARTESIAN_POINT('Ctrl Pts',(-0.229315762961314,0.0271121196187737,
-1.55348221696293));
#34416=CARTESIAN_POINT('Ctrl Pts',(-0.146925824378568,-0.178426424660404,
-1.54236443392585));
#34417=CARTESIAN_POINT('Ctrl Pts',(0.0702270199492049,-0.219974630838623,
-1.53124665088878));
#34418=CARTESIAN_POINT('Ctrl Pts',(0.222959556485836,-0.0603293268215795,
-1.52012886785171));
#34419=CARTESIAN_POINT('Ctrl Pts',(0.171531815124264,0.15472022586109,-1.50901108481464));
#34420=CARTESIAN_POINT('Ctrl Pts',(-0.0370312919934256,0.227981918373403,
-1.49789330177756));
#34421=CARTESIAN_POINT('Ctrl Pts',(-0.21166273897616,0.0924725114640206,
-1.48677551874049));
#34422=CARTESIAN_POINT('Ctrl Pts',(-0.192436817478659,-0.12775512116758,
-1.47565773570342));
#34423=CARTESIAN_POINT('Ctrl Pts',(0.00304855825315219,-0.230958843137944,
-1.46453995266635));
#34424=CARTESIAN_POINT('Ctrl Pts',(0.195739658996433,-0.122630075289071,
-1.45342216962928));
#34425=CARTESIAN_POINT('Ctrl Pts',(0.209151186357511,0.0980203721270748,
-1.4423043865922));
#34426=CARTESIAN_POINT('Ctrl Pts',(0.0309976873846526,0.228890978396746,
-1.43118660355513));
#34427=CARTESIAN_POINT('Ctrl Pts',(-0.175546722608327,0.150118035003706,
-1.42006882051806));
#34428=CARTESIAN_POINT('Ctrl Pts',(-0.221305623643101,-0.0661505383029409,
-1.40895103748099));
#34429=CARTESIAN_POINT('Ctrl Pts',(-0.0643675673818668,-0.221830684237955,
-1.39783325444391));
#34430=CARTESIAN_POINT('Ctrl Pts',(0.151525588825757,-0.174333169320765,
-1.38671547140684));
#34431=CARTESIAN_POINT('Ctrl Pts',(0.228634389855163,0.0328385665534054,
-1.37559768836977));
#34432=CARTESIAN_POINT('Ctrl Pts',(0.0963337859677596,0.209932971829016,
-1.3644799053327));
#34433=CARTESIAN_POINT('Ctrl Pts',(-0.124200255662681,0.194746889035336,
-1.35336212229563));
#34434=CARTESIAN_POINT('Ctrl Pts',(-0.230977572400255,0.00118943348492363,
-1.34224433925855));
#34435=CARTESIAN_POINT('Ctrl Pts',(-0.126199341218217,-0.193457435632643,
-1.33112655622148));
#34436=CARTESIAN_POINT('Ctrl Pts',(0.0941666072966302,-0.210913972246026,
-1.32000877318441));
#34437=CARTESIAN_POINT('Ctrl Pts',(0.228284061114703,-0.0351914895718038,
-1.30889099014733));
#34438=CARTESIAN_POINT('Ctrl Pts',(0.153312992655439,0.172763363341896,
-1.29777320711026));
#34439=CARTESIAN_POINT('Ctrl Pts',(-0.0620795614515782,0.222481867916951,
-1.28665542407319));
#34440=CARTESIAN_POINT('Ctrl Pts',(-0.22061258856118,0.0684261590905361,
-1.27553764103612));
#34441=CARTESIAN_POINT('Ctrl Pts',(-0.177083501191208,-0.148302013062266,
-1.26441985799905));
#34442=CARTESIAN_POINT('Ctrl Pts',(0.0286388087541587,-0.229198324853811,
-1.25330207496197));
#34443=CARTESIAN_POINT('Ctrl Pts',(0.208130438539744,-0.1001687278149,-1.2421842919249));
#34444=CARTESIAN_POINT('Ctrl Pts',(0.196992527342426,0.120606789400195,
-1.23106650888783));
#34445=CARTESIAN_POINT('Ctrl Pts',(0.00542644174545787,0.230916883768986,
-1.21994872585076));
#34446=CARTESIAN_POINT('Ctrl Pts',(-0.191109796735638,0.129727017504544,
-1.20883094281368));
#34447=CARTESIAN_POINT('Ctrl Pts',(-0.212605934961331,-0.0902816143971185,
-1.19771315977661));
#34448=CARTESIAN_POINT('Ctrl Pts',(-0.0393733632728863,-0.227600069735721,
-1.18659537673954));
#34449=CARTESIAN_POINT('Ctrl Pts',(0.169921815212332,-0.156456480191677,
-1.17547759370246));
#34450=CARTESIAN_POINT('Ctrl Pts',(0.223583258126262,0.0579877587484838,
-1.1643598106654));
#34451=CARTESIAN_POINT('Ctrl Pts',(0.0724617093456121,0.219320209186852,
-1.15324202762832));
#34452=CARTESIAN_POINT('Ctrl Pts',(-0.145028519037734,0.17977425328661,
-1.14212424459125));
#34453=CARTESIAN_POINT('Ctrl Pts',(-0.22968512535792,-0.0244294221862726,
-1.13100646155418));
#34454=CARTESIAN_POINT('Ctrl Pts',(-0.103969955576743,-0.20625785273878,
-1.11988867851711));
#34455=CARTESIAN_POINT('Ctrl Pts',(0.11697273136201,-0.199171869491529,
-1.10877089548003));
#34456=CARTESIAN_POINT('Ctrl Pts',(0.230778479355723,-0.00966162229131927,
-1.09765311244296));
#34457=CARTESIAN_POINT('Ctrl Pts',(0.13321103323257,0.188697838101425,-1.08653532940589));
#34458=CARTESIAN_POINT('Ctrl Pts',(-0.0863662366167158,0.21422634443902,
-1.07541754636882));
#34459=CARTESIAN_POINT('Ctrl Pts',(-0.226839478445307,0.0435419854588804,
-1.06429976333174));
#34460=CARTESIAN_POINT('Ctrl Pts',(-0.159547311451343,-0.167023078907342,
-1.05318198029467));
#34461=CARTESIAN_POINT('Ctrl Pts',(0.0538764399450253,-0.224609400288346,
-1.0420641972576));
#34462=CARTESIAN_POINT('Ctrl Pts',(0.21795401647007,-0.0764728722071082,
-1.03094641422052));
#34463=CARTESIAN_POINT('Ctrl Pts',(0.182404501420134,0.14170621489798,-1.01982863118345));
#34464=CARTESIAN_POINT('Ctrl Pts',(-0.0202118137669104,0.230094624151221,
-1.00871084814638));
#34465=CARTESIAN_POINT('Ctrl Pts',(-0.204315849790256,0.107736191706991,
-0.997593065109308));
#34466=CARTESIAN_POINT('Ctrl Pts',(-0.201284179315163,-0.113299305542715,
-0.986475282072236));
#34467=CARTESIAN_POINT('Ctrl Pts',(-0.0138935511685533,-0.230562405250654,
-0.975357499035163));
#34468=CARTESIAN_POINT('Ctrl Pts',(0.186222372232284,-0.136650216096502,
-0.964239715998091));
#34469=CARTESIAN_POINT('Ctrl Pts',(0.215774654930363,0.0824217918315482,
-0.953121932961018));
#34470=CARTESIAN_POINT('Ctrl Pts',(0.0476959533641147,0.226002543153232,
-0.942004149923947));
#34471=CARTESIAN_POINT('Ctrl Pts',(-0.164068130119753,0.162584446236557,
-0.930886366886873));
#34472=CARTESIAN_POINT('Ctrl Pts',(-0.225559948992936,-0.0497469887464949,
-0.919768583849802));
#34473=CARTESIAN_POINT('Ctrl Pts',(-0.0804582977272316,-0.216514470199744,
-0.908650800812729));
#34474=CARTESIAN_POINT('Ctrl Pts',(0.138336218797355,-0.18497336037357,
-0.897533017775658));
#34475=CARTESIAN_POINT('Ctrl Pts',(0.230426683406532,0.0159874029568902,
-0.886415234738584));
#34476=CARTESIAN_POINT('Ctrl Pts',(0.111466168663688,0.202305083283833,
-0.875297451701513));
#34477=CARTESIAN_POINT('Ctrl Pts',(-0.109587748255086,0.203328745905295,
-0.864179668664439));
#34478=CARTESIAN_POINT('Ctrl Pts',(-0.230268734173445,0.0181208040991509,
-0.853061885627368));
#34479=CARTESIAN_POINT('Ctrl Pts',(-0.140043408622157,-0.183684232258863,
-0.841944102590293));
#34480=CARTESIAN_POINT('Ctrl Pts',(0.0784496075652732,-0.217250345343557,
-0.830826319553223));
#34481=CARTESIAN_POINT('Ctrl Pts',(0.225089545534232,-0.0518338689491085,
-0.819708536516149));
#34482=CARTESIAN_POINT('Ctrl Pts',(0.165566862383964,0.161057963352855,
-0.808590753479078));
#34483=CARTESIAN_POINT('Ctrl Pts',(-0.0456007949411382,0.22643458432796,
-0.797472970442004));
#34484=CARTESIAN_POINT('Ctrl Pts',(-0.215002054862611,0.084416644590361,
-0.786355187404934));
#34485=CARTESIAN_POINT('Ctrl Pts',(-0.187479965584133,-0.134919664925512,
-0.77523740436786));
#34486=CARTESIAN_POINT('Ctrl Pts',(0.0117576115035681,-0.230681191367592,
-0.764119621330788));
#34487=CARTESIAN_POINT('Ctrl Pts',(0.200226229953391,-0.115158631103761,
-0.753001838293715));
#34488=CARTESIAN_POINT('Ctrl Pts',(0.205304881152449,0.105839308642956,
-0.741884055256644));
#34489=CARTESIAN_POINT('Ctrl Pts',(0.0223419583792376,0.229897564960615,
-0.73076627221957));
#34490=CARTESIAN_POINT('Ctrl Pts',(-0.181084272405317,0.143389468813009,
-0.719648489182499));
#34491=CARTESIAN_POINT('Ctrl Pts',(-0.21865291902735,-0.0744510206770842,
-0.708530706145426));
#34492=CARTESIAN_POINT('Ctrl Pts',(-0.0559543395769349,-0.224100792862384,
-0.697412923108353));
#34493=CARTESIAN_POINT('Ctrl Pts',(0.157993591693872,-0.168493556145955,
-0.686295140071281));
#34494=CARTESIAN_POINT('Ctrl Pts',(0.227233011930364,0.0414392539519657,
-0.675177357034209));
#34495=CARTESIAN_POINT('Ctrl Pts',(0.0883465805943492,0.213417279469883,
-0.664059573997136));
#34496=CARTESIAN_POINT('Ctrl Pts',(-0.131457703141354,0.189923473440857,
-0.652941790960065));
#34497=CARTESIAN_POINT('Ctrl Pts',(-0.230858062378427,-0.00752386296517325,
-0.64182400792299));
#34498=CARTESIAN_POINT('Ctrl Pts',(-0.118812336309844,-0.19807998944779,
-0.630706224885921));
#34499=CARTESIAN_POINT('Ctrl Pts',(0.102055248263095,-0.20721191997807,
-0.619588441848847));
#34500=CARTESIAN_POINT('Ctrl Pts',(0.229449022531091,-0.0265555933574688,
-0.608470658811775));
#34501=CARTESIAN_POINT('Ctrl Pts',(0.146687270535163,0.178423367701611,
-0.597352875774702));
#34502=CARTESIAN_POINT('Ctrl Pts',(-0.0704273769121229,0.219981903938297,
-0.58623509273763));
#34503=CARTESIAN_POINT('Ctrl Pts',(-0.223036617907527,0.0600559784818474,
-0.575117309700557));
#34504=CARTESIAN_POINT('Ctrl Pts',(-0.171363542528578,-0.154876046472966,
-0.563999526663486));
#34505=CARTESIAN_POINT('Ctrl Pts',(0.0372637663671585,-0.227954963085198,
-0.552881743626412));
#34506=CARTESIAN_POINT('Ctrl Pts',(0.211760677385933,-0.0922467830988746,
-0.541763960589341));
#34507=CARTESIAN_POINT('Ctrl Pts',(0.192303061568511,0.127951498586056,
-0.530646177552267));
#34508=CARTESIAN_POINT('Ctrl Pts',(-0.00328758223170905,0.230957236912183,
-0.519528394515196));
#34509=CARTESIAN_POINT('Ctrl Pts',(-0.195867084095393,0.122426054608521,
-0.508410611478123));
#34510=CARTESIAN_POINT('Ctrl Pts',(-0.209049220558358,-0.0982368406606357,
-0.497292828441051));
#34511=CARTESIAN_POINT('Ctrl Pts',(-0.0307602909131559,-0.228923257844148,
-0.486175045403978));
#34512=CARTESIAN_POINT('Ctrl Pts',(0.175702413689009,-0.14993570389636,
-0.475057262366906));
#34513=CARTESIAN_POINT('Ctrl Pts',(0.221236852799642,0.0663800304485451,
-0.463939479329834));
#34514=CARTESIAN_POINT('Ctrl Pts',(0.0641374052360248,0.221897378823251,
-0.452821696292761));
#34515=CARTESIAN_POINT('Ctrl Pts',(-0.151706376916133,0.174175855623051,
-0.441703913255688));
#34516=CARTESIAN_POINT('Ctrl Pts',(-0.228600194816059,-0.0330757374687038,
-0.430586130218617));
#34517=CARTESIAN_POINT('Ctrl Pts',(-0.0961159394705803,-0.210032806148765,
-0.419468347181543));
#34518=CARTESIAN_POINT('Ctrl Pts',(0.124402231290949,-0.194617929104401,
-0.408350564144472));
#34519=CARTESIAN_POINT('Ctrl Pts',(0.230978681591128,-0.000949804954544109,
-0.397232781107399));
#34520=CARTESIAN_POINT('Ctrl Pts',(0.125998569784222,0.193588258660883,
-0.386114998070328));
#34521=CARTESIAN_POINT('Ctrl Pts',(-0.094385370940541,0.210816164540436,
-0.374997215033254));
#34522=CARTESIAN_POINT('Ctrl Pts',(-0.228320447848423,0.034954635933263,
-0.363879431996183));
#34523=CARTESIAN_POINT('Ctrl Pts',(-0.153133675619892,-0.172922326118124,
-0.352761648959109));
#34524=CARTESIAN_POINT('Ctrl Pts',(0.062310343442467,-0.2224173432529,-0.341643865922038));
#34525=CARTESIAN_POINT('Ctrl Pts',(0.22068345902505,-0.0681972462121358,
-0.330526082884965));
#34526=CARTESIAN_POINT('Ctrl Pts',(0.176929548933351,0.148485649788263,
-0.319408299847893));
#34527=CARTESIAN_POINT('Ctrl Pts',(-0.0288765767642302,0.229168489974145,
-0.30829051681082));
#34528=CARTESIAN_POINT('Ctrl Pts',(-0.208234247273263,0.0999527475109843,
-0.297172733773748));
#34529=CARTESIAN_POINT('Ctrl Pts',(-0.196867296985244,-0.120811095753957,
-0.286054950736675));
#34530=CARTESIAN_POINT('Ctrl Pts',(-0.00518687244590196,-0.230922389248131,
-0.274937167699603));
#34531=CARTESIAN_POINT('Ctrl Pts',(0.191244280031821,-0.129528679392947,
-0.263819384662531));
#34532=CARTESIAN_POINT('Ctrl Pts',(0.212512157369943,0.090502135153134,
-0.252701601625458));
#34533=CARTESIAN_POINT('Ctrl Pts',(0.0391372165612645,0.227640795768667,
-0.241583818588386));
#34534=CARTESIAN_POINT('Ctrl Pts',(-0.170084040207984,0.156280108753479,
-0.230466035551313));
#34535=CARTESIAN_POINT('Ctrl Pts',(-0.223522978823559,-0.0582196843152984,
-0.219348252514241));
#34536=CARTESIAN_POINT('Ctrl Pts',(-0.0722341334783348,-0.219395269448206,
-0.208230469477168));
#34537=CARTESIAN_POINT('Ctrl Pts',(0.145214946051373,-0.1796236911522,-0.197112686440096));
#34538=CARTESIAN_POINT('Ctrl Pts',(0.229659662987761,0.0246676888676773,
-0.185994903403024));
#34539=CARTESIAN_POINT('Ctrl Pts',(0.103755905091973,0.206365622507627,
-0.174877120365952));
#34540=CARTESIAN_POINT('Ctrl Pts',(-0.117179279978873,0.199050376899346,
-0.163759337328879));
#34541=CARTESIAN_POINT('Ctrl Pts',(-0.230788418054293,0.00942225375522446,
-0.152641554291807));
#34542=CARTESIAN_POINT('Ctrl Pts',(-0.13301512070789,-0.188836050358411,
-0.141523771254734));
#34543=CARTESIAN_POINT('Ctrl Pts',(0.086588298155162,-0.214136412684086,
-0.130405988217662));
#34544=CARTESIAN_POINT('Ctrl Pts',(0.226884800711301,-0.0433070353739192,
-0.11928820518059));
#34545=CARTESIAN_POINT('Ctrl Pts',(0.159373429816203,0.167189291936005,
-0.108170422143517));
#34546=CARTESIAN_POINT('Ctrl Pts',(-0.0541084505942859,0.224551901584748,
-0.0970526391064448));
#34547=CARTESIAN_POINT('Ctrl Pts',(-0.218035107164092,0.0762495360628558,
-0.0859348560693726));
#34548=CARTESIAN_POINT('Ctrl Pts',(-0.182253829063119,-0.141900747845757,
-0.0748170730323));
#34549=CARTESIAN_POINT('Ctrl Pts',(0.0204437407985646,-0.230063306839836,
-0.0636992899952277));
#34550=CARTESIAN_POINT('Ctrl Pts',(0.204440407371902,-0.107543627072653,
-0.0525815069581553));
#34551=CARTESIAN_POINT('Ctrl Pts',(0.201141971358471,0.113545140191613,
-0.041463723921083));
#34552=CARTESIAN_POINT('Ctrl Pts',(0.0137012025830432,0.230505855872065,
-0.0303459408840108));
#34553=CARTESIAN_POINT('Ctrl Pts',(-0.186454285750881,0.136594239305857,
-0.0192281578469384));
#34554=CARTESIAN_POINT('Ctrl Pts',(-0.215508026917975,-0.0829281406198991,
-0.00811037480986591));
#34555=CARTESIAN_POINT('Ctrl Pts',(-0.103761961485765,-0.177874731816565,
-0.000698519451817671));
#34556=CARTESIAN_POINT('Ctrl Pts',(-0.0401504189376247,-0.191230499291126,
0.00300740822720647));
#34557=CARTESIAN_POINT('Ctrl Pts',(-0.195211655640432,0.00014838930625368,
-0.0821869692124233));
#34558=CARTESIAN_POINT('Ctrl Pts',(-0.194905158848201,-0.0430319431973475,
-0.0797303371523822));
#34559=CARTESIAN_POINT('Ctrl Pts',(-0.18078209130478,-0.0863940405347896,
-0.0772737050923411));
#34560=CARTESIAN_POINT('Ctrl Pts',(-0.154434447103001,-0.120236127026668,
-0.0748170730323));
#34561=CARTESIAN_POINT('Ctrl Pts',(-0.114687972442558,-0.17128826751045,
-0.0711111453532758));
#34562=CARTESIAN_POINT('Ctrl Pts',(-0.0471221158219972,-0.200675787175143,
-0.0674052176742518));
#34563=CARTESIAN_POINT('Ctrl Pts',(0.0173269235838404,-0.194949600379625,
-0.0636992899952276));
#34564=CARTESIAN_POINT('Ctrl Pts',(0.0817759629896761,-0.189223413584108,
-0.0599933623162036));
#34565=CARTESIAN_POINT('Ctrl Pts',(0.143108185180787,-0.148383520328383,
-0.0562874346371796));
#34566=CARTESIAN_POINT('Ctrl Pts',(0.173224556940772,-0.0911154458231427,
-0.0525815069581555));
#34567=CARTESIAN_POINT('Ctrl Pts',(0.203340928700759,-0.0338473713179008,
-0.0488755792791313));
#34568=CARTESIAN_POINT('Ctrl Pts',(0.202241450029616,0.0398488844368553,
-0.0451696516001073));
#34569=CARTESIAN_POINT('Ctrl Pts',(0.170451582564806,0.0961904649276424,
-0.0414637239210832));
#34570=CARTESIAN_POINT('Ctrl Pts',(0.138661715099997,0.152532045418428,
-0.0377577962420592));
#34571=CARTESIAN_POINT('Ctrl Pts',(0.0761814588415184,0.191518950645247,
-0.0340518685630348));
#34572=CARTESIAN_POINT('Ctrl Pts',(0.0115820826566276,0.195360467164288,
-0.0303459408840108));
#34573=CARTESIAN_POINT('Ctrl Pts',(-0.0485325395593545,0.198935289831578,
-0.0268972939226739));
#34574=CARTESIAN_POINT('Ctrl Pts',(-0.110482259223248,0.172075207744509,
-0.0234486469613371));
#34575=CARTESIAN_POINT('Ctrl Pts',(-0.149578925757925,0.126231591330479,
-0.0200000000000002));
#34576=CARTESIAN_POINT('',(-0.0903606778650182,-0.126612599672285,-1.5646));
#34577=CARTESIAN_POINT('Ctrl Pts',(-0.0905548925879826,-0.126791816255572,
-1.5646));
#34578=CARTESIAN_POINT('Ctrl Pts',(-0.0937532001918452,-0.125081815778544,
-1.5646));
#34579=CARTESIAN_POINT('Ctrl Pts',(-0.0968817208862554,-0.123255435291712,
-1.5646));
#34580=CARTESIAN_POINT('Ctrl Pts',(-0.0999333552098715,-0.121314098198218,
-1.5646));
#34581=CARTESIAN_POINT('Ctrl Pts',(-0.107358826195873,-0.116590287697651,
-1.5646));
#34582=CARTESIAN_POINT('Ctrl Pts',(-0.114329742086453,-0.111187533769295,
-1.5646));
#34583=CARTESIAN_POINT('Ctrl Pts',(-0.120819049765463,-0.10520686979309,
-1.5646));
#34584=CARTESIAN_POINT('Ctrl Pts',(-0.123912141625436,-0.102356220081739,
-1.5646));
#34585=CARTESIAN_POINT('Ctrl Pts',(-0.126895620400741,-0.0993734486954757,
-1.5646));
#34586=CARTESIAN_POINT('Ctrl Pts',(-0.129756065809199,-0.0962799395198511,
-1.5646));
#34587=CARTESIAN_POINT('Ctrl Pts',(-0.13505492992586,-0.0905493338187916,
-1.5646));
#34588=CARTESIAN_POINT('Ctrl Pts',(-0.139941342179991,-0.0844312047867337,
-1.5646));
#34589=CARTESIAN_POINT('Ctrl Pts',(-0.144395973511904,-0.0779901114787239,
-1.5646));
#34590=CARTESIAN_POINT('Ctrl Pts',(-0.146717425902047,-0.0746334495372757,
-1.5646));
#34591=CARTESIAN_POINT('Ctrl Pts',(-0.148922318893028,-0.0711875248212428,
-1.5646));
#34592=CARTESIAN_POINT('Ctrl Pts',(-0.151004655746733,-0.0676646554325792,
-1.5646));
#34593=CARTESIAN_POINT('Ctrl Pts',(-0.156939281662135,-0.0576245353946859,
-1.5646));
#34594=CARTESIAN_POINT('Ctrl Pts',(-0.161845187410773,-0.0470244648230485,
-1.5646));
#34595=CARTESIAN_POINT('Ctrl Pts',(-0.165663065915722,-0.0360640028289907,
-1.5646));
#34596=CARTESIAN_POINT('Ctrl Pts',(-0.168575860309324,-0.0277018791505693,
-1.5646));
#34597=CARTESIAN_POINT('Ctrl Pts',(-0.170855019541254,-0.0191286573412821,
-1.5646));
#34598=CARTESIAN_POINT('Ctrl Pts',(-0.172459025338206,-0.0104201269361194,
-1.5646));
#34599=CARTESIAN_POINT('Ctrl Pts',(-0.173099136546176,-0.00694481037062258,
-1.5646));
#34600=CARTESIAN_POINT('Ctrl Pts',(-0.173631215439875,-0.00344800373498262,
-1.5646));
#34601=CARTESIAN_POINT('Ctrl Pts',(-0.174051082244989,5.13592542474017E-5,
-1.5646));
#34602=CARTESIAN_POINT('Ctrl Pts',(-0.174868285791271,0.00686230932149219,
-1.5646));
#34603=CARTESIAN_POINT('Ctrl Pts',(-0.175263381326914,0.0136958974655043,
-1.5646));
#34604=CARTESIAN_POINT('Ctrl Pts',(-0.175222363933104,0.0205158229853707,
-1.5646));
#34605=CARTESIAN_POINT('Ctrl Pts',(-0.175176056838249,0.0282152623845594,
-1.5646));
#34606=CARTESIAN_POINT('Ctrl Pts',(-0.174574248416374,0.035897416489142,
-1.5646));
#34607=CARTESIAN_POINT('Ctrl Pts',(-0.173452468406207,0.0435229784332608,
-1.5646));
#34608=CARTESIAN_POINT('Ctrl Pts',(-0.172769676803301,0.0481644140228602,
-1.5646));
#34609=CARTESIAN_POINT('Ctrl Pts',(-0.171894043795892,0.0527849303693672,
-1.5646));
#34610=CARTESIAN_POINT('Ctrl Pts',(-0.170831789993684,0.0573757738448648,
-1.5646));
#34611=CARTESIAN_POINT('Ctrl Pts',(-0.1700259113612,0.060858616320261,-1.5646));
#34612=CARTESIAN_POINT('Ctrl Pts',(-0.169112472680126,0.0643237115920012,
-1.5646));
#34613=CARTESIAN_POINT('Ctrl Pts',(-0.168098483581223,0.0677542609967512,
-1.5646));
#34614=CARTESIAN_POINT('Ctrl Pts',(-0.164843308212733,0.0787672392771043,
-1.5646));
#34615=CARTESIAN_POINT('Ctrl Pts',(-0.160547607684451,0.0894588682215987,
-1.5646));
#34616=CARTESIAN_POINT('Ctrl Pts',(-0.15532132364043,0.0997061301383391,
-1.5646));
#34617=CARTESIAN_POINT('Ctrl Pts',(-0.152112604778659,0.105997518497027,
-1.5646));
#34618=CARTESIAN_POINT('Ctrl Pts',(-0.14855224829291,0.112121534649242,
-1.5646));
#34619=CARTESIAN_POINT('Ctrl Pts',(-0.144658388961414,0.11804872209353,
-1.5646));
#34620=CARTESIAN_POINT('Ctrl Pts',(-0.141735673513408,0.122497645598941,
-1.5646));
#34621=CARTESIAN_POINT('Ctrl Pts',(-0.138620900433489,0.126840131680051,
-1.5646));
#34622=CARTESIAN_POINT('Ctrl Pts',(-0.135341984423439,0.131036730447831,
-1.5646));
#34623=CARTESIAN_POINT('Ctrl Pts',(-0.127445990316296,0.141142606609001,
-1.5646));
#34624=CARTESIAN_POINT('Ctrl Pts',(-0.118587414130911,0.150430178036819,
-1.5646));
#34625=CARTESIAN_POINT('Ctrl Pts',(-0.108883967809866,0.158736266807026,
-1.5646));
#34626=CARTESIAN_POINT('Ctrl Pts',(-0.101753616243006,0.16483980271763,
-1.5646));
#34627=CARTESIAN_POINT('Ctrl Pts',(-0.0941658812525659,0.170413396666743,
-1.5646));
#34628=CARTESIAN_POINT('Ctrl Pts',(-0.0861525859670562,0.175382131162753,
-1.5646));
#34629=CARTESIAN_POINT('Ctrl Pts',(-0.0905548925879821,-0.126791816255572,
-1.5646));
#34630=CARTESIAN_POINT('Ctrl Pts',(-0.0513799502789448,-0.154465111057779,
-1.56115135303866));
#34631=CARTESIAN_POINT('Ctrl Pts',(0.058718500965293,-0.172171894665568,
-1.5539967783983));
#34632=CARTESIAN_POINT('Ctrl Pts',(0.177489043046939,-0.0480257256248533,
-1.54313627607892));
#34633=CARTESIAN_POINT('Ctrl Pts',(0.136549507894468,0.123166484814191,
-1.53201849304185));
#34634=CARTESIAN_POINT('Ctrl Pts',(-0.0294791068043894,0.181487141263986,
-1.52090071000477));
#34635=CARTESIAN_POINT('Ctrl Pts',(-0.141282213466497,0.0947308729275798,
-1.51195933813737));
#34636=CARTESIAN_POINT('Ctrl Pts',(-0.155414140615138,0.0214996094033827,
-1.50672389394899));
#34637=CARTESIAN_POINT('Ctrl Pts',(-0.155325699155423,7.24743171158018E-5,
-1.50519437743963));
#34638=CARTESIAN_POINT('Origin',(-2.59090492670967E-17,0.,-1.5646));
#34639=CARTESIAN_POINT('',(-0.1954,-2.39295984553393E-17,-1.5646));
#34640=CARTESIAN_POINT('Origin',(0.,0.,-1.5646));
#34641=CARTESIAN_POINT('Origin',(0.,0.,-1.5646));
#34642=CARTESIAN_POINT('',(0.0903606778650233,-0.126612599672282,-1.5646));
#34643=CARTESIAN_POINT('Ctrl Pts',(0.0863567411264547,0.175643900344958,
-1.5646));
#34644=CARTESIAN_POINT('Ctrl Pts',(0.0901946439528806,0.173286650680855,
-1.5646));
#34645=CARTESIAN_POINT('Ctrl Pts',(0.0939395416005596,0.170790644243054,
-1.5646));
#34646=CARTESIAN_POINT('Ctrl Pts',(0.0975828366931286,0.168155421712109,
-1.5646));
#34647=CARTESIAN_POINT('Ctrl Pts',(0.104715013233486,0.162996665191902,
-1.5646));
#34648=CARTESIAN_POINT('Ctrl Pts',(0.111458438257504,0.157304747156973,
-1.5646));
#34649=CARTESIAN_POINT('Ctrl Pts',(0.1177825331303,0.151141812734413,-1.5646));
#34650=CARTESIAN_POINT('Ctrl Pts',(0.120981747064298,0.148024126160198,
-1.5646));
#34651=CARTESIAN_POINT('Ctrl Pts',(0.124075275555252,0.144783758201481,
-1.5646));
#34652=CARTESIAN_POINT('Ctrl Pts',(0.127052171083901,0.14143511287228,-1.5646));
#34653=CARTESIAN_POINT('Ctrl Pts',(0.135245602155662,0.13221849965071,-1.5646));
#34654=CARTESIAN_POINT('Ctrl Pts',(0.142538985144231,0.122207558577474,
-1.5646));
#34655=CARTESIAN_POINT('Ctrl Pts',(0.14884096310014,0.111572087435399,-1.5646));
#34656=CARTESIAN_POINT('Ctrl Pts',(0.150925188381918,0.10805466512878,-1.5646));
#34657=CARTESIAN_POINT('Ctrl Pts',(0.152901721781693,0.104466619547691,
-1.5646));
#34658=CARTESIAN_POINT('Ctrl Pts',(0.154762551889738,0.10082101919008,-1.5646));
#34659=CARTESIAN_POINT('Ctrl Pts',(0.160363871395494,0.0898473293808975,
-1.5646));
#34660=CARTESIAN_POINT('Ctrl Pts',(0.164897520476248,0.0784015119881915,
-1.5646));
#34661=CARTESIAN_POINT('Ctrl Pts',(0.168269747317322,0.0666527387236212,
-1.5646));
#34662=CARTESIAN_POINT('Ctrl Pts',(0.17053544204992,0.0587591019801492,
-1.5646));
#34663=CARTESIAN_POINT('Ctrl Pts',(0.172275892452234,0.0507282896369748,
-1.5646));
#34664=CARTESIAN_POINT('Ctrl Pts',(0.173448974571123,0.0426121852966646,
-1.5646));
#34665=CARTESIAN_POINT('Ctrl Pts',(0.174147941571219,0.0377763012508139,
-1.5646));
#34666=CARTESIAN_POINT('Ctrl Pts',(0.174645109427981,0.0329053571363106,
-1.5646));
#34667=CARTESIAN_POINT('Ctrl Pts',(0.174929105367026,0.0280403292564174,
-1.5646));
#34668=CARTESIAN_POINT('Ctrl Pts',(0.175316356965979,0.021406467406935,
-1.5646));
#34669=CARTESIAN_POINT('Ctrl Pts',(0.175309624504317,0.0147741099420037,
-1.5646));
#34670=CARTESIAN_POINT('Ctrl Pts',(0.174889543081871,0.00817125191888272,
-1.5646));
#34671=CARTESIAN_POINT('Ctrl Pts',(0.174139516163367,-0.00361770372585117,
-1.5646));
#34672=CARTESIAN_POINT('Ctrl Pts',(0.172074020516654,-0.0153146206873486,
-1.5646));
#34673=CARTESIAN_POINT('Ctrl Pts',(0.168782371632102,-0.0267416672032861,
-1.5646));
#34674=CARTESIAN_POINT('Ctrl Pts',(0.167753283826731,-0.0303141728481449,
-1.5646));
#34675=CARTESIAN_POINT('Ctrl Pts',(0.166603407781752,-0.0338609610831103,
-1.5646));
#34676=CARTESIAN_POINT('Ctrl Pts',(0.165341255244092,-0.0373603852761497,
-1.5646));
#34677=CARTESIAN_POINT('Ctrl Pts',(0.161969828859879,-0.0467079488248741,
-1.5646));
#34678=CARTESIAN_POINT('Ctrl Pts',(0.157791865228321,-0.0557463282631995,
-1.5646));
#34679=CARTESIAN_POINT('Ctrl Pts',(0.152867464919401,-0.0643714118638176,
-1.5646));
#34680=CARTESIAN_POINT('Ctrl Pts',(0.150136227847812,-0.0691551716310509,
-1.5646));
#34681=CARTESIAN_POINT('Ctrl Pts',(0.147174947330489,-0.0738115070429787,
-1.5646));
#34682=CARTESIAN_POINT('Ctrl Pts',(0.14399136084734,-0.0783197279550166,
-1.5646));
#34683=CARTESIAN_POINT('Ctrl Pts',(0.142004455648795,-0.0811333495147673,
-1.5646));
#34684=CARTESIAN_POINT('Ctrl Pts',(0.139930928123689,-0.0838892324174092,
-1.5646));
#34685=CARTESIAN_POINT('Ctrl Pts',(0.137772411698158,-0.0865818092317733,
-1.5646));
#34686=CARTESIAN_POINT('Ctrl Pts',(0.135523663129691,-0.0893869434365289,
-1.5646));
#34687=CARTESIAN_POINT('Ctrl Pts',(0.133187545061614,-0.0921171125955211,
-1.5646));
#34688=CARTESIAN_POINT('Ctrl Pts',(0.130770515703773,-0.0947630325834097,
-1.5646));
#34689=CARTESIAN_POINT('Ctrl Pts',(0.123527059508787,-0.102692437936115,
-1.5646));
#34690=CARTESIAN_POINT('Ctrl Pts',(0.115548451594148,-0.109881057155588,
-1.5646));
#34691=CARTESIAN_POINT('Ctrl Pts',(0.10689716230252,-0.116171310827943,
-1.5646));
#34692=CARTESIAN_POINT('Ctrl Pts',(0.101630903118588,-0.120000347755809,
-1.5646));
#34693=CARTESIAN_POINT('Ctrl Pts',(0.0961149067122779,-0.123495713824771,
-1.5646));
#34694=CARTESIAN_POINT('Ctrl Pts',(0.0903606778650246,-0.126612599672281,
-1.5646));
#34695=CARTESIAN_POINT('Origin',(0.,0.,-1.5646));
#34696=CARTESIAN_POINT('Origin',(0.,0.,-1.69400562256037));
#34697=CARTESIAN_POINT('Ctrl Pts',(0.0903606778650232,-0.126612599672282,
-1.5646));
#34698=CARTESIAN_POINT('Ctrl Pts',(0.132477509652,-0.0965547264460079,-1.56089407232098));
#34699=CARTESIAN_POINT('Ctrl Pts',(0.183629629053462,0.00837163889085661,
-1.55348221696293));
#34700=CARTESIAN_POINT('Ctrl Pts',(0.0923230570238932,0.159158029769189,
-1.54236443392586));
#34701=CARTESIAN_POINT('Ctrl Pts',(-0.0836206488085049,0.163699342626539,
-1.53124665088878));
#34702=CARTESIAN_POINT('Ctrl Pts',(-0.153174468253431,0.0620393558697811,
-1.52346038043362));
#34703=CARTESIAN_POINT('Ctrl Pts',(-0.155774899534441,0.00530901775232087,
-1.51938003765748));
#34704=CARTESIAN_POINT('Ctrl Pts',(-0.155739242772632,9.98782012467418E-5,
-1.51900562256037));
#34705=CARTESIAN_POINT('Ctrl Pts',(0.113509973994377,-0.159049193030949,
-1.58760740822721));
#34706=CARTESIAN_POINT('Ctrl Pts',(0.166416620932181,-0.121290861765029,
-1.58390148054818));
#34707=CARTESIAN_POINT('Ctrl Pts',(0.230673285226915,0.0105163499792544,
-1.57648962519013));
#34708=CARTESIAN_POINT('Ctrl Pts',(0.11597509059768,0.199932362693021,-1.56537184215306));
#34709=CARTESIAN_POINT('Ctrl Pts',(-0.105043232254462,0.205637104141601,
-1.55425405911599));
#34710=CARTESIAN_POINT('Ctrl Pts',(-0.229800035323766,0.0232923379007898,
-1.54313627607892));
#34711=CARTESIAN_POINT('Ctrl Pts',(-0.144106605593727,-0.180540291081365,
-1.53201849304185));
#34712=CARTESIAN_POINT('Ctrl Pts',(0.0735901299731223,-0.218932805076657,
-1.52090071000477));
#34713=CARTESIAN_POINT('Ctrl Pts',(0.223877253749246,-0.0568441566047822,
-1.5097829269677));
#34714=CARTESIAN_POINT('Ctrl Pts',(0.169115997122617,0.157331121656424,
-1.49866514393063));
#34715=CARTESIAN_POINT('Ctrl Pts',(-0.0405429768310065,0.227392947574501,
-1.48754736089356));
#34716=CARTESIAN_POINT('Ctrl Pts',(-0.213067006103068,0.0891885853239147,
-1.47642957785648));
#34717=CARTESIAN_POINT('Ctrl Pts',(-0.190440587625236,-0.13070806461951,
-1.46531179481941));
#34718=CARTESIAN_POINT('Ctrl Pts',(0.00661328935441616,-0.23088569648881,
-1.45419401178234));
#34719=CARTESIAN_POINT('Ctrl Pts',(0.197609807773384,-0.119592824631789,
-1.44307622874526));
#34720=CARTESIAN_POINT('Ctrl Pts',(0.207612857862459,0.101237234431652,
-1.43195844570819));
#34721=CARTESIAN_POINT('Ctrl Pts',(0.0274603833141874,0.229342467105821,
-1.42084066267112));
#34722=CARTESIAN_POINT('Ctrl Pts',(-0.177843412717356,0.14738989847531,
-1.40972287963405));
#34723=CARTESIAN_POINT('Ctrl Pts',(-0.220257984554934,-0.0695591802067529,
-1.39860509659698));
#34724=CARTESIAN_POINT('Ctrl Pts',(-0.0609352224241326,-0.222798010068075,
-1.38748731355991));
#34725=CARTESIAN_POINT('Ctrl Pts',(0.154198947593458,-0.171973086531601,
-1.37636953052283));
#34726=CARTESIAN_POINT('Ctrl Pts',(0.228100175195862,0.0363643701443694,
-1.36525174748576));
#34727=CARTESIAN_POINT('Ctrl Pts',(0.093081303520226,0.211395193176495,
-1.35413396444868));
#34728=CARTESIAN_POINT('Ctrl Pts',(-0.127192018150192,0.192806244125044,
-1.34301618141162));
#34729=CARTESIAN_POINT('Ctrl Pts',(-0.230968415323631,-0.00237660618670745,
-1.33189839837454));
#34730=CARTESIAN_POINT('Ctrl Pts',(-0.123197653274959,-0.195382689342334,
-1.32078061533747));
#34731=CARTESIAN_POINT('Ctrl Pts',(0.0974115395374693,-0.209435071331169,
-1.3096628323004));
#34732=CARTESIAN_POINT('Ctrl Pts',(0.228800158988753,-0.0316629809566973,
-1.29854504926333));
#34733=CARTESIAN_POINT('Ctrl Pts',(0.150627555230227,0.175109670534308,
-1.28742726622625));
#34734=CARTESIAN_POINT('Ctrl Pts',(-0.0655069051000644,0.221496958226608,
-1.27630948318918));
#34735=CARTESIAN_POINT('Ctrl Pts',(-0.221642687021708,0.0650121250644202,
-1.26519170015211));
#34736=CARTESIAN_POINT('Ctrl Pts',(-0.174772873101609,-0.151018210632965,
-1.25407391711503));
#34737=CARTESIAN_POINT('Ctrl Pts',(0.0321738272563805,-0.228728883082269,
-1.24295613407796));
#34738=CARTESIAN_POINT('Ctrl Pts',(0.209652075213801,-0.0969436149227984,
-1.23183835104089));
#34739=CARTESIAN_POINT('Ctrl Pts',(0.195107094163994,0.123633648019485,
-1.22072056800382));
#34740=CARTESIAN_POINT('Ctrl Pts',(0.00186083298014342,0.230973146526896,
-1.20960278496674));
#34741=CARTESIAN_POINT('Ctrl Pts',(-0.193089790810889,0.12676115256821,
-1.19848500192967));
#34742=CARTESIAN_POINT('Ctrl Pts',(-0.21118681044866,-0.0935531304037486,
-1.1873672188926));
#34743=CARTESIAN_POINT('Ctrl Pts',(-0.0358549158978023,-0.228180810152399,
-1.17624943585553));
#34744=CARTESIAN_POINT('Ctrl Pts',(0.172316990942207,-0.153814536856734,
-1.16513165281846));
#34745=CARTESIAN_POINT('Ctrl Pts',(0.222661387705244,0.0614325934745175,
-1.15401386978138));
#34746=CARTESIAN_POINT('Ctrl Pts',(0.0690671466145953,0.22041276363757,
-1.14289608674431));
#34747=CARTESIAN_POINT('Ctrl Pts',(-0.147786647226476,0.1775138417628,-1.13177830370724));
#34748=CARTESIAN_POINT('Ctrl Pts',(-0.229280611332588,-0.027972457575022,
-1.12066052067017));
#34749=CARTESIAN_POINT('Ctrl Pts',(-0.100773299315656,-0.207838396983976,
-1.10954273763309));
#34750=CARTESIAN_POINT('Ctrl Pts',(0.120033668273633,-0.197342280306596,
-1.09842495459602));
#34751=CARTESIAN_POINT('Ctrl Pts',(0.23090014255785,-0.00609764566010633,
-1.08730717155895));
#34752=CARTESIAN_POINT('Ctrl Pts',(0.130281989719349,0.190731906797471,
-1.07618938852188));
#34753=CARTESIAN_POINT('Ctrl Pts',(-0.0896632354690507,0.212867473609881,
-1.0650716054848));
#34754=CARTESIAN_POINT('Ctrl Pts',(-0.227484665887432,0.0400347836501573,
-1.05395382244773));
#34755=CARTESIAN_POINT('Ctrl Pts',(-0.156949751401061,-0.169466317157649,
-1.04283603941066));
#34756=CARTESIAN_POINT('Ctrl Pts',(0.0573376063898475,-0.223750879348696,
-1.03171825637359));
#34757=CARTESIAN_POINT('Ctrl Pts',(0.219108659196544,-0.0730989232542078,
-1.02060047333651));
#34758=CARTESIAN_POINT('Ctrl Pts',(0.180195067220354,0.144505345455744,
-1.00948269029944));
#34759=CARTESIAN_POINT('Ctrl Pts',(-0.0237616736179114,0.229755174006392,
-0.99836490726237));
#34760=CARTESIAN_POINT('Ctrl Pts',(-0.205954769664849,0.104569067931823,
-0.987247124225297));
#34761=CARTESIAN_POINT('Ctrl Pts',(-0.199511049882178,-0.116393290574426,
-0.976129341188227));
#34762=CARTESIAN_POINT('Ctrl Pts',(-0.0103324061458603,-0.230749427949602,
-0.965011558151152));
#34763=CARTESIAN_POINT('Ctrl Pts',(0.188309830972563,-0.1337589797917,-0.953893775114082));
#34764=CARTESIAN_POINT('Ctrl Pts',(0.214476495119882,0.0857431639078181,
-0.942775992077007));
#34765=CARTESIAN_POINT('Ctrl Pts',(0.0442011774886412,0.22671196047948,
-0.931658209039936));
#34766=CARTESIAN_POINT('Ctrl Pts',(-0.166558608605968,0.160032143693309,
-0.920540426002863));
#34767=CARTESIAN_POINT('Ctrl Pts',(-0.224765066474341,-0.0532233220366446,
-0.909422642965791));
#34768=CARTESIAN_POINT('Ctrl Pts',(-0.0771060980724411,-0.21773081260096,
-0.898304859928718));
#34769=CARTESIAN_POINT('Ctrl Pts',(0.141175409662247,-0.182815647094357,
-0.887187076891647));
#34770=CARTESIAN_POINT('Ctrl Pts',(0.230152411385913,0.0195428925464229,
-0.876069293854574));
#34771=CARTESIAN_POINT('Ctrl Pts',(0.108329643286355,0.204001827200844,
-0.864951510817501));
#34772=CARTESIAN_POINT('Ctrl Pts',(-0.112713740110191,0.201612672980158,
-0.85383372778043));
#34773=CARTESIAN_POINT('Ctrl Pts',(-0.230521053425755,0.0145636892067859,
-0.842715944743356));
#34774=CARTESIAN_POINT('Ctrl Pts',(-0.137190952586333,-0.185824378498318,
-0.831598161706284));
#34775=CARTESIAN_POINT('Ctrl Pts',(0.0817942350404951,-0.216013333454145,
-0.820480378669212));
#34776=CARTESIAN_POINT('Ctrl Pts',(0.225862953986525,-0.0483526951918151,
-0.80936259563214));
#34777=CARTESIAN_POINT('Ctrl Pts',(0.163060676338395,0.163594843891539,
-0.798244812595066));
#34778=CARTESIAN_POINT('Ctrl Pts',(-0.0490911250986347,0.225703607752251,
-0.787127029557995));
#34779=CARTESIAN_POINT('Ctrl Pts',(-0.216279687572231,0.0810873224338431,
-0.776009246520923));
#34780=CARTESIAN_POINT('Ctrl Pts',(-0.185374699415074,-0.137797960553133,
-0.764891463483849));
#34781=CARTESIAN_POINT('Ctrl Pts',(0.0153175342131884,-0.230472189778852,
-0.753773680446778));
#34782=CARTESIAN_POINT('Ctrl Pts',(0.201980226864861,-0.112053759738131,
-0.742655897409705));
#34783=CARTESIAN_POINT('Ctrl Pts',(0.203646442288396,0.108996255252695,
-0.731538114372633));
#34784=CARTESIAN_POINT('Ctrl Pts',(0.0187900707826508,0.230215095846938,
-0.720420331335561));
#34785=CARTESIAN_POINT('Ctrl Pts',(-0.183276385866645,0.140576753055022,
-0.709302548298488));
#34786=CARTESIAN_POINT('Ctrl Pts',(-0.217477471381767,-0.0778177778995558,
-0.698184765261416));
#34787=CARTESIAN_POINT('Ctrl Pts',(-0.0524879395448804,-0.224937932146103,
-0.687066982224343));
#34788=CARTESIAN_POINT('Ctrl Pts',(0.160576020484737,-0.166034330067962,
-0.675949199187271));
#34789=CARTESIAN_POINT('Ctrl Pts',(0.226566187311492,0.0449424062881105,
-0.664831416150198));
#34790=CARTESIAN_POINT('Ctrl Pts',(0.0850412564367271,0.214755772493999,
-0.653713633113127));
#34791=CARTESIAN_POINT('Ctrl Pts',(-0.134374134826396,0.187871362920188,
-0.642595850076053));
#34792=CARTESIAN_POINT('Ctrl Pts',(-0.230714401562136,-0.0110870206844455,
-0.631478067038982));
#34793=CARTESIAN_POINT('Ctrl Pts',(-0.115740163916463,-0.199890649036972,
-0.620360284001908));
#34794=CARTESIAN_POINT('Ctrl Pts',(0.105242087140735,-0.205611673331291,
-0.609242500964837));
#34795=CARTESIAN_POINT('Ctrl Pts',(0.229831658184759,-0.0230101284628302,
-0.598124717927765));
#34796=CARTESIAN_POINT('Ctrl Pts',(0.143915241689072,0.180666710617666,
-0.587006934890691));
#34797=CARTESIAN_POINT('Ctrl Pts',(-0.0738151307822532,0.218868416139539,
-0.575889151853619));
#34798=CARTESIAN_POINT('Ctrl Pts',(-0.223937206279105,0.056605518809929,
-0.564771368816547));
#34799=CARTESIAN_POINT('Ctrl Pts',(-0.168952104083443,-0.157503154386219,
-0.553653585779474));
#34800=CARTESIAN_POINT('Ctrl Pts',(0.0407785618778789,-0.227352514846447,
-0.542535802742403));
#34801=CARTESIAN_POINT('Ctrl Pts',(0.213159580247783,-0.08896656936412,
-0.531418019705329));
#34802=CARTESIAN_POINT('Ctrl Pts',(0.190304797344661,0.130905084788328,
-0.520300236668258));
#34803=CARTESIAN_POINT('Ctrl Pts',(-0.00685277576144637,0.230878965218131,
-0.509182453631185));
#34804=CARTESIAN_POINT('Ctrl Pts',(-0.197733796975422,0.119387615142923,
-0.498064670594113));
#34805=CARTESIAN_POINT('Ctrl Pts',(-0.207507704700154,-0.101452499259039,
-0.48694688755704));
#34806=CARTESIAN_POINT('Ctrl Pts',(-0.027222441965051,-0.229370869487148,
-0.475829104519968));
#34807=CARTESIAN_POINT('Ctrl Pts',(0.177996231051109,-0.147205294902844,
-0.464711321482895));
#34808=CARTESIAN_POINT('Ctrl Pts',(0.220185699597794,0.0697876408002185,
-0.453593538445824));
#34809=CARTESIAN_POINT('Ctrl Pts',(0.0607040471943301,0.222861113184999,
-0.44247575540875));
#34810=CARTESIAN_POINT('Ctrl Pts',(-0.154377279785012,0.171813016392891,
-0.431357972371679));
#34811=CARTESIAN_POINT('Ctrl Pts',(-0.228062325714473,-0.0366009932313942,
-0.420240189334605));
#34812=CARTESIAN_POINT('Ctrl Pts',(-0.0928619401316778,-0.211491648040283,
-0.409122406297534));
#34813=CARTESIAN_POINT('Ctrl Pts',(0.127391977965817,-0.19267418370366,
-0.398004623260461));
#34814=CARTESIAN_POINT('Ctrl Pts',(0.230965825361851,0.00261622450151,-0.386886840223389));
#34815=CARTESIAN_POINT('Ctrl Pts',(0.122994885849355,0.195510396579458,
-0.375769057186316));
#34816=CARTESIAN_POINT('Ctrl Pts',(-0.0976287670138966,0.209333898276729,
-0.364651274149244));
#34817=CARTESIAN_POINT('Ctrl Pts',(-0.228832884833302,0.0314255936116178,
-0.353533491112171));
#34818=CARTESIAN_POINT('Ctrl Pts',(-0.150445805414977,-0.175265845927362,
-0.3424157080751));
#34819=CARTESIAN_POINT('Ctrl Pts',(0.0657366634319771,-0.221428878424336,
-0.331297925038026));
#34820=CARTESIAN_POINT('Ctrl Pts',(0.221710015017261,-0.0647821453049757,
-0.320180142000955));
#34821=CARTESIAN_POINT('Ctrl Pts',(0.17461610416282,0.151199448687295,-0.309062358963882));
#34822=CARTESIAN_POINT('Ctrl Pts',(-0.0324111063717073,0.22869538106904,
-0.29794457592681));
#34823=CARTESIAN_POINT('Ctrl Pts',(-0.209752537145294,0.096726057648452,
-0.286826792889737));
#34824=CARTESIAN_POINT('Ctrl Pts',(-0.194978724715305,-0.123835996553786,
-0.275709009852665));
#34825=CARTESIAN_POINT('Ctrl Pts',(-0.00162120698158336,-0.230974953063417,
-0.264591226815592));
#34826=CARTESIAN_POINT('Ctrl Pts',(0.193221195612131,-0.126560761412732,
-0.253473443778521));
#34827=CARTESIAN_POINT('Ctrl Pts',(0.211089640462245,0.0937721762032856,
-0.242355660741447));
#34828=CARTESIAN_POINT('Ctrl Pts',(0.0356181668760191,0.228217887376357,
-0.231237877704376));
#34829=CARTESIAN_POINT('Ctrl Pts',(-0.172476470490578,0.153635678633855,
-0.220120094667302));
#34830=CARTESIAN_POINT('Ctrl Pts',(-0.222597541227211,-0.0616635544778054,
-0.209002311630231));
#34831=CARTESIAN_POINT('Ctrl Pts',(-0.0688384273015429,-0.220484313605681,
-0.197884528593158));
#34832=CARTESIAN_POINT('Ctrl Pts',(0.147970705227284,-0.177360396550321,
-0.186766745556086));
#34833=CARTESIAN_POINT('Ctrl Pts',(0.22925151616086,0.0282102591823235,
-0.175648962519013));
#34834=CARTESIAN_POINT('Ctrl Pts',(0.100557529478573,0.207942932307904,
-0.164531179481941));
#34835=CARTESIAN_POINT('Ctrl Pts',(-0.120238162331385,0.197217455511372,
-0.153413396444869));
#34836=CARTESIAN_POINT('Ctrl Pts',(-0.23090667834121,0.00585845278655507,
-0.142295613407796));
#34837=CARTESIAN_POINT('Ctrl Pts',(-0.130083407741252,-0.19086765014593,
-0.131177830370724));
#34838=CARTESIAN_POINT('Ctrl Pts',(0.0898828181189855,-0.212773035377908,
-0.120060047333651));
#34839=CARTESIAN_POINT('Ctrl Pts',(0.227528380768991,-0.0398012345171181,
-0.108942264296579));
#34840=CARTESIAN_POINT('Ctrl Pts',(0.156769469656559,0.16963377101867,-0.0978244812595063));
#34841=CARTESIAN_POINT('Ctrl Pts',(-0.0575613644483651,0.223682296329051,
-0.086706698222434));
#34842=CARTESIAN_POINT('Ctrl Pts',(-0.219200259963039,0.0728886583195608,
-0.0755889151853618));
#34843=CARTESIAN_POINT('Ctrl Pts',(-0.18001480464987,-0.144724771019191,
-0.0644711321482894));
#34844=CARTESIAN_POINT('Ctrl Pts',(0.023942282457509,-0.229668165736859,
-0.0533533491112173));
#34845=CARTESIAN_POINT('Ctrl Pts',(0.206174498061778,-0.104476062522128,
-0.0422355660741447));
#34846=CARTESIAN_POINT('Ctrl Pts',(0.199165675931825,0.11684944015648,-0.0311177830370723));
#34847=CARTESIAN_POINT('Ctrl Pts',(0.0734746804820682,0.192373169122532,
-0.0237059276790242));
#34848=CARTESIAN_POINT('Ctrl Pts',(0.00853826423429785,0.19521336543348,
-0.02));
#34849=CARTESIAN_POINT('Ctrl Pts',(0.105793541951259,-0.148236995244726,
-1.57993827215147));
#34850=CARTESIAN_POINT('Ctrl Pts',(0.155103583838787,-0.113045483325355,
-1.57623234447245));
#34851=CARTESIAN_POINT('Ctrl Pts',(0.214992066502431,0.00980144628312182,
-1.5688204891144));
#34852=CARTESIAN_POINT('Ctrl Pts',(0.108091079406417,0.186340918385077,
-1.55770270607733));
#34853=CARTESIAN_POINT('Ctrl Pts',(-0.0979023711058095,0.191657850303247,
-1.54658492304025));
#34854=CARTESIAN_POINT('Ctrl Pts',(-0.214178180312418,0.0217089198432209,
-1.53546714000318));
#34855=CARTESIAN_POINT('Ctrl Pts',(-0.134310208062321,-0.168267123903623,
-1.52434935696611));
#34856=CARTESIAN_POINT('Ctrl Pts',(0.06858745737089,-0.204049706676274,
-1.51323157392904));
#34857=CARTESIAN_POINT('Ctrl Pts',(0.208658030682192,-0.0529798788144361,
-1.50211379089197));
#34858=CARTESIAN_POINT('Ctrl Pts',(0.157619455864793,0.146635718725669,
-1.49099600785489));
#34859=CARTESIAN_POINT('Ctrl Pts',(-0.0377868566899024,0.211934726897524,
-1.47987822481782));
#34860=CARTESIAN_POINT('Ctrl Pts',(-0.198582665957713,0.0831255264273637,
-1.46876044178075));
#34861=CARTESIAN_POINT('Ctrl Pts',(-0.177494396194213,-0.121822502737751,
-1.45764265874368));
#34862=CARTESIAN_POINT('Ctrl Pts',(0.00616371654518196,-0.215190038001811,
-1.4465248757066));
#34863=CARTESIAN_POINT('Ctrl Pts',(0.184176251240171,-0.111462879115622,
-1.43540709266953));
#34864=CARTESIAN_POINT('Ctrl Pts',(0.193499291868227,0.0943551058200843,
-1.42428930963246));
#34865=CARTESIAN_POINT('Ctrl Pts',(0.0255936206477411,0.213751717678719,
-1.41317152659539));
#34866=CARTESIAN_POINT('Ctrl Pts',(-0.165753579901275,0.137370301999293,
-1.40205374355831));
#34867=CARTESIAN_POINT('Ctrl Pts',(-0.2052848001733,-0.0648305324223128,
-1.39093596052124));
#34868=CARTESIAN_POINT('Ctrl Pts',(-0.056792833113996,-0.207652154214761,
-1.37981817748417));
#34869=CARTESIAN_POINT('Ctrl Pts',(0.143716470518058,-0.160282319731389,
-1.3687003944471));
#34870=CARTESIAN_POINT('Ctrl Pts',(0.212593877035584,0.0338923125697315,
-1.35758261141002));
#34871=CARTESIAN_POINT('Ctrl Pts',(0.0867536168172552,0.19702450322753,
-1.34646482837295));
#34872=CARTESIAN_POINT('Ctrl Pts',(-0.118545477851173,0.179699234864752,
-1.33534704533588));
#34873=CARTESIAN_POINT('Ctrl Pts',(-0.215267133592743,-0.00221504399540788,
-1.32422926229881));
#34874=CARTESIAN_POINT('Ctrl Pts',(-0.114822650745093,-0.18210053279117,
-1.31311147926173));
#34875=CARTESIAN_POINT('Ctrl Pts',(0.0907894824740647,-0.195197630879878,
-1.30199369622466));
#34876=CARTESIAN_POINT('Ctrl Pts',(0.213246275782165,-0.0295105248135298,
-1.29087591318759));
#34877=CARTESIAN_POINT('Ctrl Pts',(0.140387862163143,0.163205678090104,
-1.27975813015052));
#34878=CARTESIAN_POINT('Ctrl Pts',(-0.0610537318345626,0.206439548152691,
-1.26864034711344));
#34879=CARTESIAN_POINT('Ctrl Pts',(-0.206575370273473,0.0605925870504019,
-1.25752256407637));
#34880=CARTESIAN_POINT('Ctrl Pts',(-0.162891776218123,-0.140751960728968,
-1.2464047810393));
#34881=CARTESIAN_POINT('Ctrl Pts',(0.0299866436737017,-0.213179845226881,
-1.23528699800223));
#34882=CARTESIAN_POINT('Ctrl Pts',(0.195399882792665,-0.0903533674736788,
-1.22416921496516));
#34883=CARTESIAN_POINT('Ctrl Pts',(0.181843672631351,0.115229006474661,
-1.21305143192808));
#34884=CARTESIAN_POINT('Ctrl Pts',(0.00173433316052722,0.215271543167809,
-1.20193364889101));
#34885=CARTESIAN_POINT('Ctrl Pts',(-0.179963505986915,0.118143902602595,
-1.19081586585394));
#34886=CARTESIAN_POINT('Ctrl Pts',(-0.196830286401612,-0.0871933688094308,
-1.17969808281686));
#34887=CARTESIAN_POINT('Ctrl Pts',(-0.0334174911306108,-0.212669030410719,
-1.16858029977979));
#34888=CARTESIAN_POINT('Ctrl Pts',(0.160602845447415,-0.143358192104532,
-1.15746251674272));
#34889=CARTESIAN_POINT('Ctrl Pts',(0.207524819469055,0.057256392775167,
-1.14634473370565));
#34890=CARTESIAN_POINT('Ctrl Pts',(0.06437194737783,0.205429057341158,-1.13522695066858));
#34891=CARTESIAN_POINT('Ctrl Pts',(-0.13774007968643,0.165446413249924,
-1.1241091676315));
#34892=CARTESIAN_POINT('Ctrl Pts',(-0.213694066874035,-0.0260708839920053,
-1.11299138459443));
#34893=CARTESIAN_POINT('Ctrl Pts',(-0.0939227091114099,-0.193709498792555,
-1.10187360155736));
#34894=CARTESIAN_POINT('Ctrl Pts',(0.111873754113442,-0.183926910347166,
-1.09075581852029));
#34895=CARTESIAN_POINT('Ctrl Pts',(0.215203502024021,-0.00568312641828513,
-1.07963803548321));
#34896=CARTESIAN_POINT('Ctrl Pts',(0.12142539249943,0.177765911427496,-1.06852025244614));
#34897=CARTESIAN_POINT('Ctrl Pts',(-0.0835679097552307,0.19839669772562,
-1.05740246940907));
#34898=CARTESIAN_POINT('Ctrl Pts',(-0.212020210180141,0.0373132105889854,
-1.04628468637199));
#34899=CARTESIAN_POINT('Ctrl Pts',(-0.146280274100937,-0.15794596106974,
-1.03516690333492));
#34900=CARTESIAN_POINT('Ctrl Pts',(0.0534397837787334,-0.208540247240122,
-1.02404912029785));
#34901=CARTESIAN_POINT('Ctrl Pts',(0.204213606195892,-0.0681296429886322,
-1.01293133726078));
#34902=CARTESIAN_POINT('Ctrl Pts',(0.167945368433709,0.134681841504173,
-1.00181355422371));
#34903=CARTESIAN_POINT('Ctrl Pts',(-0.0221463500190146,0.214136368676889,
-0.990695771186635));
#34904=CARTESIAN_POINT('Ctrl Pts',(-0.191953920857029,0.0974604405741237,
-0.979577988149561));
#34905=CARTESIAN_POINT('Ctrl Pts',(-0.185948246508236,-0.108480850060283,
-0.968460205112491));
#34906=CARTESIAN_POINT('Ctrl Pts',(-0.0096300069904304,-0.215063033026724,
-0.957342422075416));
#34907=CARTESIAN_POINT('Ctrl Pts',(0.175508488829512,-0.124666016051169,
-0.946224639038346));
#34908=CARTESIAN_POINT('Ctrl Pts',(0.199896337613012,0.0799143254879507,
-0.935106856001272));
#34909=CARTESIAN_POINT('Ctrl Pts',(0.0411963720930036,0.211300033449274,
-0.923989072964201));
#34910=CARTESIAN_POINT('Ctrl Pts',(-0.155235919160475,0.149153124713134,
-0.912871289927127));
#34911=CARTESIAN_POINT('Ctrl Pts',(-0.209485489710434,-0.0496051893461636,
-0.901753506890056));
#34912=CARTESIAN_POINT('Ctrl Pts',(-0.0718644092150764,-0.202929425903335,
-0.890635723852983));
#34913=CARTESIAN_POINT('Ctrl Pts',(0.131578275450305,-0.170387800733541,
-0.879517940815911));
#34914=CARTESIAN_POINT('Ctrl Pts',(0.214506601775322,0.0182143625771726,
-0.868400157778838));
#34915=CARTESIAN_POINT('Ctrl Pts',(0.100965371220572,0.190133739834837,
-0.857282374741766));
#34916=CARTESIAN_POINT('Ctrl Pts',(-0.105051436214949,0.187907000823454,
-0.846164591704694));
#34917=CARTESIAN_POINT('Ctrl Pts',(-0.214850183451316,0.0135736465338231,
-0.835046808667621));
#34918=CARTESIAN_POINT('Ctrl Pts',(-0.12786468260925,-0.173191997940219,
-0.82392902563055));
#34919=CARTESIAN_POINT('Ctrl Pts',(0.0762338456403528,-0.201328701352221,
-0.812811242593475));
#34920=CARTESIAN_POINT('Ctrl Pts',(0.210508742597301,-0.0450656687445377,
-0.801693459556405));
#34921=CARTESIAN_POINT('Ctrl Pts',(0.151975777068376,0.152473631798264,
-0.79057567651933));
#34922=CARTESIAN_POINT('Ctrl Pts',(-0.0457539000300912,0.210360228753739,
-0.77945789348226));
#34923=CARTESIAN_POINT('Ctrl Pts',(-0.201576948661017,0.0755749891022346,
-0.768340110445186));
#34924=CARTESIAN_POINT('Ctrl Pts',(-0.172772888136174,-0.128430426046067,
-0.757222327408115));
#34925=CARTESIAN_POINT('Ctrl Pts',(0.0142762449972293,-0.214804641565465,
-0.746104544371042));
#34926=CARTESIAN_POINT('Ctrl Pts',(0.188249568317327,-0.104436321448188,
-0.73498676133397));
#34927=CARTESIAN_POINT('Ctrl Pts',(0.189802514063912,0.101586666764432,
-0.723868978296898));
#34928=CARTESIAN_POINT('Ctrl Pts',(0.0175127177961463,0.214565024933426,
-0.712751195259824));
#34929=CARTESIAN_POINT('Ctrl Pts',(-0.170817218386628,0.131020315645873,
-0.701633412222753));
#34930=CARTESIAN_POINT('Ctrl Pts',(-0.202693306873811,-0.0725277088970024,
-0.69051562918568));
#34931=CARTESIAN_POINT('Ctrl Pts',(-0.0489197983117454,-0.209646603937262,
-0.679397846148608));
#34932=CARTESIAN_POINT('Ctrl Pts',(0.149660028645235,-0.154747281188384,
-0.668280063111535));
#34933=CARTESIAN_POINT('Ctrl Pts',(0.211164169972081,0.041887212001893,
-0.657162280074463));
#34934=CARTESIAN_POINT('Ctrl Pts',(0.0792601338352194,0.20015662965216,
-0.646044497037391));
#34935=CARTESIAN_POINT('Ctrl Pts',(-0.125239352716482,0.175099827928087,
-0.634926714000318));
#34936=CARTESIAN_POINT('Ctrl Pts',(-0.215030387740486,-0.0103333226730591,
-0.623808930963246));
#34937=CARTESIAN_POINT('Ctrl Pts',(-0.107872123090684,-0.18630204043219,
-0.612691147926174));
#34938=CARTESIAN_POINT('Ctrl Pts',(0.0980877077948493,-0.191634148284802,
-0.6015733648891));
#34939=CARTESIAN_POINT('Ctrl Pts',(0.214207653444632,-0.0214458950625499,
-0.590455581852029));
#34940=CARTESIAN_POINT('Ctrl Pts',(0.134131853116384,0.168384949413105,
-0.579337798814955));
#34941=CARTESIAN_POINT('Ctrl Pts',(-0.0687971625774212,0.203989694912721,
-0.568220015777885));
#34942=CARTESIAN_POINT('Ctrl Pts',(-0.208713907626388,0.0527574636673564,
-0.557102232740811));
#34943=CARTESIAN_POINT('Ctrl Pts',(-0.157466704309091,-0.146796056634102,
-0.545984449703739));
#34944=CARTESIAN_POINT('Ctrl Pts',(0.0380064266154546,-0.211897042794876,
-0.534866666666667));
#34945=CARTESIAN_POINT('Ctrl Pts',(0.198668946892488,-0.0829186031594792,
-0.523748883629593));
#34946=CARTESIAN_POINT('Ctrl Pts',(0.177367836965635,0.122006129433817,
-0.512631100592523));
#34947=CARTESIAN_POINT('Ctrl Pts',(-0.00638692261560318,0.215183764324336,
-0.501513317555449));
#34948=CARTESIAN_POINT('Ctrl Pts',(-0.184291811630027,0.111271619811218,
-0.490395534518377));
#34949=CARTESIAN_POINT('Ctrl Pts',(-0.193401287040138,-0.09455573689897,
-0.479277751481305));
#34950=CARTESIAN_POINT('Ctrl Pts',(-0.0253718546018513,-0.213778189260156,
-0.468159968444233));
#34951=CARTESIAN_POINT('Ctrl Pts',(0.165896009612375,-0.137198247816732,
-0.457042185407159));
#34952=CARTESIAN_POINT('Ctrl Pts',(0.205217429162836,0.065043462216308,
-0.445924402370089));
#34953=CARTESIAN_POINT('Ctrl Pts',(0.0565773732252167,0.207710967568448,
-0.434806619333014));
#34954=CARTESIAN_POINT('Ctrl Pts',(-0.143882679649508,0.160133131194568,
-0.423688836295944));
#34955=CARTESIAN_POINT('Ctrl Pts',(-0.212558600569946,-0.0341128499692469,
-0.41257105325887));
#34956=CARTESIAN_POINT('Ctrl Pts',(-0.0865491657982631,-0.197114401069274,
-0.401453270221798));
#34957=CARTESIAN_POINT('Ctrl Pts',(0.118731844356234,-0.179576151938748,
-0.390335487184726));
#34958=CARTESIAN_POINT('Ctrl Pts',(0.215264719697113,0.00243837300648307,
-0.379217704147653));
#34959=CARTESIAN_POINT('Ctrl Pts',(0.114633667491973,0.182219558463301,
-0.368099921110581));
#34960=CARTESIAN_POINT('Ctrl Pts',(-0.0909919427806939,0.19510333559108,
-0.356982138073508));
#34961=CARTESIAN_POINT('Ctrl Pts',(-0.213276776916879,0.0292892751103837,
-0.345864355036436));
#34962=CARTESIAN_POINT('Ctrl Pts',(-0.140218467738779,-0.163351236646902,
-0.334746571999364));
#34963=CARTESIAN_POINT('Ctrl Pts',(0.0612678711464706,-0.206376096429779,
-0.323628788962291));
#34964=CARTESIAN_POINT('Ctrl Pts',(0.206638121297647,-0.0603782413636525,
-0.312511005925219));
#34965=CARTESIAN_POINT('Ctrl Pts',(0.162745664464955,0.140920878182027,
-0.301393222888146));
#34966=CARTESIAN_POINT('Ctrl Pts',(-0.0302077925045763,0.213148620687599,
-0.290275439851075));
#34967=CARTESIAN_POINT('Ctrl Pts',(-0.195493515300804,0.0901505997888629,
-0.279157656814001));
#34968=CARTESIAN_POINT('Ctrl Pts',(-0.181724029764938,-0.115417599312797,
-0.26803987377693));
#34969=CARTESIAN_POINT('Ctrl Pts',(-0.0015109969880378,-0.215273226895595,
-0.256922090739857));
#34970=CARTESIAN_POINT('Ctrl Pts',(0.180085977861972,-0.117957134080256,
-0.245804307702785));
#34971=CARTESIAN_POINT('Ctrl Pts',(0.196739722051428,0.08739752382918,-0.234686524665712));
#34972=CARTESIAN_POINT('Ctrl Pts',(0.0331968363574083,0.212703587117149,
-0.22356874162864));
#34973=CARTESIAN_POINT('Ctrl Pts',(-0.160751483542354,0.143191492701478,
-0.212450958591567));
#34974=CARTESIAN_POINT('Ctrl Pts',(-0.207465313288104,-0.0574716530005959,
-0.201333175554495));
#34975=CARTESIAN_POINT('Ctrl Pts',(-0.0641587764520602,-0.205495743327301,
-0.190215392517423));
#34976=CARTESIAN_POINT('Ctrl Pts',(0.137911625385409,-0.165303399275447,
-0.17909760948035));
#34977=CARTESIAN_POINT('Ctrl Pts',(0.213666949598236,0.02629251979574,-0.167979826443278));
#34978=CARTESIAN_POINT('Ctrl Pts',(0.0937216073534937,0.19380692778305,
-0.156862043406205));
#34979=CARTESIAN_POINT('Ctrl Pts',(-0.112064346621891,0.183810571167925,
-0.145744260369133));
#34980=CARTESIAN_POINT('Ctrl Pts',(-0.215209593503446,0.00546019392687473,
-0.134626477332061));
#34981=CARTESIAN_POINT('Ctrl Pts',(-0.121240310166211,-0.177892426914413,
-0.123508694294988));
#34982=CARTESIAN_POINT('Ctrl Pts',(0.0837725651301739,-0.198308679424633,
-0.112390911257916));
#34983=CARTESIAN_POINT('Ctrl Pts',(0.212060953314804,-0.0370955381754129,
-0.101273128220843));
#34984=CARTESIAN_POINT('Ctrl Pts',(0.146112247947562,0.158102031381867,
-0.090155345183771));
#34985=CARTESIAN_POINT('Ctrl Pts',(-0.0536483307171008,0.208476326508661,
-0.0790375621466985));
#34986=CARTESIAN_POINT('Ctrl Pts',(-0.204298979922905,0.0679336719087199,
-0.0679197791096263));
#34987=CARTESIAN_POINT('Ctrl Pts',(-0.167777360150897,-0.134886350471401,
-0.0568019960725539));
#34988=CARTESIAN_POINT('Ctrl Pts',(0.0223146810314913,-0.214055275247924,
-0.0456842130354818));
#34989=CARTESIAN_POINT('Ctrl Pts',(0.192158712071056,-0.0973737576918526,
-0.0345664299984093));
#34990=CARTESIAN_POINT('Ctrl Pts',(0.185626351152085,0.108905990497259,
-0.0234486469613368));
#34991=CARTESIAN_POINT('Ctrl Pts',(0.0684798561606579,0.179295600392521,
-0.0160367916032887));
#34992=CARTESIAN_POINT('Ctrl Pts',(0.0079578312255345,0.181942719557458,
-0.0123308639242645));
#34993=CARTESIAN_POINT('Ctrl Pts',(0.098077109908141,-0.137424797458504,
-1.57226913607574));
#34994=CARTESIAN_POINT('Ctrl Pts',(0.143790546745394,-0.104800104885681,
-1.56856320839671));
#34995=CARTESIAN_POINT('Ctrl Pts',(0.199310847777946,0.00908654258698918,
-1.56115135303866));
#34996=CARTESIAN_POINT('Ctrl Pts',(0.100207068215156,0.172749474077133,
-1.55003357000159));
#34997=CARTESIAN_POINT('Ctrl Pts',(-0.0907615099571574,0.177678596464893,
-1.53891578696452));
#34998=CARTESIAN_POINT('Ctrl Pts',(-0.19855632530107,0.0201255017856523,
-1.52779800392744));
#34999=CARTESIAN_POINT('Ctrl Pts',(-0.124513810530915,-0.155993956725882,
-1.51668022089038));
#35000=CARTESIAN_POINT('Ctrl Pts',(0.0635847847686578,-0.18916660827589,
-1.5055624378533));
#35001=CARTESIAN_POINT('Ctrl Pts',(0.193438807615137,-0.0491156010240898,
-1.49444465481623));
#35002=CARTESIAN_POINT('Ctrl Pts',(0.146122914606969,0.135940315794915,
-1.48332687177916));
#35003=CARTESIAN_POINT('Ctrl Pts',(-0.0350307365487982,0.196476506220547,
-1.47220908874208));
#35004=CARTESIAN_POINT('Ctrl Pts',(-0.184098325812358,0.0770624675308122,
-1.46109130570501));
#35005=CARTESIAN_POINT('Ctrl Pts',(-0.16454820476319,-0.112936940855992,
-1.44997352266794));
#35006=CARTESIAN_POINT('Ctrl Pts',(0.00571414373594752,-0.199494379514811,
-1.43885573963087));
#35007=CARTESIAN_POINT('Ctrl Pts',(0.170742694706959,-0.103332933599455,
-1.42773795659379));
#35008=CARTESIAN_POINT('Ctrl Pts',(0.179385725873994,0.0874729772085164,
-1.41662017355672));
#35009=CARTESIAN_POINT('Ctrl Pts',(0.0237268579812951,0.198160968251618,
-1.40550239051965));
#35010=CARTESIAN_POINT('Ctrl Pts',(-0.153663747085195,0.127350705523275,
-1.39438460748258));
#35011=CARTESIAN_POINT('Ctrl Pts',(-0.190311615791665,-0.0601018846378727,
-1.38326682444551));
#35012=CARTESIAN_POINT('Ctrl Pts',(-0.0526504438038595,-0.192506298361447,
-1.37214904140843));
#35013=CARTESIAN_POINT('Ctrl Pts',(0.133233993442659,-0.148591552931176,
-1.36103125837136));
#35014=CARTESIAN_POINT('Ctrl Pts',(0.197087578875306,0.0314202549950935,
-1.34991347533429));
#35015=CARTESIAN_POINT('Ctrl Pts',(0.0804259301142846,0.182653813278565,
-1.33879569229721));
#35016=CARTESIAN_POINT('Ctrl Pts',(-0.109898937552154,0.16659222560446,
-1.32767790926015));
#35017=CARTESIAN_POINT('Ctrl Pts',(-0.199565851861855,-0.00205348180410804,
-1.31656012622307));
#35018=CARTESIAN_POINT('Ctrl Pts',(-0.106447648215227,-0.168818376240007,
-1.305442343186));
#35019=CARTESIAN_POINT('Ctrl Pts',(0.0841674254106597,-0.180960190428586,
-1.29432456014892));
#35020=CARTESIAN_POINT('Ctrl Pts',(0.197692392575578,-0.0273580686703621,
-1.28320677711186));
#35021=CARTESIAN_POINT('Ctrl Pts',(0.130148169096058,0.151301685645901,
-1.27208899407478));
#35022=CARTESIAN_POINT('Ctrl Pts',(-0.0566005585690605,0.191382138078774,
-1.26097121103771));
#35023=CARTESIAN_POINT('Ctrl Pts',(-0.191508053525239,0.0561730490363835,
-1.24985342800064));
#35024=CARTESIAN_POINT('Ctrl Pts',(-0.151010679334637,-0.13048571082497,
-1.23873564496356));
#35025=CARTESIAN_POINT('Ctrl Pts',(0.0277994600910228,-0.197630807371493,
-1.22761786192649));
#35026=CARTESIAN_POINT('Ctrl Pts',(0.181147690371529,-0.0837631200245593,
-1.21650007888942));
#35027=CARTESIAN_POINT('Ctrl Pts',(0.168580251098708,0.106824364929836,
-1.20538229585234));
#35028=CARTESIAN_POINT('Ctrl Pts',(0.00160783334091074,0.199569939808722,
-1.19426451281528));
#35029=CARTESIAN_POINT('Ctrl Pts',(-0.166837221162941,0.10952665263698,
-1.1831467297782));
#35030=CARTESIAN_POINT('Ctrl Pts',(-0.182473762354565,-0.080833607215113,
-1.17202894674113));
#35031=CARTESIAN_POINT('Ctrl Pts',(-0.0309800663634189,-0.197157250669039,
-1.16091116370406));
#35032=CARTESIAN_POINT('Ctrl Pts',(0.148888699952624,-0.132901847352329,
-1.14979338066698));
#35033=CARTESIAN_POINT('Ctrl Pts',(0.192388251232866,0.0530801920758167,
-1.13867559762991));
#35034=CARTESIAN_POINT('Ctrl Pts',(0.0596767481410642,0.190445351044745,
-1.12755781459284));
#35035=CARTESIAN_POINT('Ctrl Pts',(-0.127693512146385,0.153378984737048,
-1.11644003155577));
#35036=CARTESIAN_POINT('Ctrl Pts',(-0.198107522415482,-0.0241693104089889,
-1.1053222485187));
#35037=CARTESIAN_POINT('Ctrl Pts',(-0.0870721189071633,-0.179580600601133,
-1.09420446548162));
#35038=CARTESIAN_POINT('Ctrl Pts',(0.103713839953251,-0.170511540387736,
-1.08308668244455));
#35039=CARTESIAN_POINT('Ctrl Pts',(0.199506861490193,-0.00526860717646393,
-1.07196889940748));
#35040=CARTESIAN_POINT('Ctrl Pts',(0.112568795279511,0.164799916057522,
-1.06085111637041));
#35041=CARTESIAN_POINT('Ctrl Pts',(-0.0774725840414104,0.183925921841359,
-1.04973333333333));
#35042=CARTESIAN_POINT('Ctrl Pts',(-0.19655575447285,0.0345916375278131,
-1.03861555029626));
#35043=CARTESIAN_POINT('Ctrl Pts',(-0.135610796800813,-0.146425604981832,
-1.02749776725919));
#35044=CARTESIAN_POINT('Ctrl Pts',(0.0495419611676193,-0.193329615131549,
-1.01637998422212));
#35045=CARTESIAN_POINT('Ctrl Pts',(0.18931855319524,-0.0631603627230562,
-1.00526220118505));
#35046=CARTESIAN_POINT('Ctrl Pts',(0.155695669647064,0.124858337552601,
-0.99414441814797));
#35047=CARTESIAN_POINT('Ctrl Pts',(-0.0205310264201175,0.198517563347386,
-0.9830266351109));
#35048=CARTESIAN_POINT('Ctrl Pts',(-0.177953072049209,0.0903518132164242,
-0.971908852073826));
#35049=CARTESIAN_POINT('Ctrl Pts',(-0.172385443134293,-0.100568409546141,
-0.960791069036755));
#35050=CARTESIAN_POINT('Ctrl Pts',(-0.00892760783500083,-0.199376638103845,
-0.949673285999682));
#35051=CARTESIAN_POINT('Ctrl Pts',(0.162707146686461,-0.115573052310637,
-0.938555502962609));
#35052=CARTESIAN_POINT('Ctrl Pts',(0.185316180106141,0.0740854870680833,
-0.927437719925537));
#35053=CARTESIAN_POINT('Ctrl Pts',(0.0381915666973661,0.195888106419067,
-0.916319936888465));
#35054=CARTESIAN_POINT('Ctrl Pts',(-0.143913229714983,0.138274105732958,
-0.905202153851392));
#35055=CARTESIAN_POINT('Ctrl Pts',(-0.194205912946527,-0.0459870566556826,
-0.89408437081432));
#35056=CARTESIAN_POINT('Ctrl Pts',(-0.0666227203577119,-0.188128039205709,
-0.882966587777248));
#35057=CARTESIAN_POINT('Ctrl Pts',(0.121981141238363,-0.157959954372725,
-0.871848804740174));
#35058=CARTESIAN_POINT('Ctrl Pts',(0.19886079216473,0.0168858326079224,
-0.860731021703104));
#35059=CARTESIAN_POINT('Ctrl Pts',(0.0936010991547904,0.176265652468829,
-0.84961323866603));
#35060=CARTESIAN_POINT('Ctrl Pts',(-0.0973891323197074,0.174201328666751,
-0.838495455628959));
#35061=CARTESIAN_POINT('Ctrl Pts',(-0.199179313476877,0.0125836038608601,
-0.827377672591885));
#35062=CARTESIAN_POINT('Ctrl Pts',(-0.118538412632168,-0.160559617382119,
-0.816259889554814));
#35063=CARTESIAN_POINT('Ctrl Pts',(0.0706734562402105,-0.186644069250297,
-0.80514210651774));
#35064=CARTESIAN_POINT('Ctrl Pts',(0.195154531208078,-0.0417786422972597,
-0.794024323480671));
#35065=CARTESIAN_POINT('Ctrl Pts',(0.140890877798356,0.14135241970499,-0.782906540443595));
#35066=CARTESIAN_POINT('Ctrl Pts',(-0.0424166749615475,0.195016849755228,
-0.771788757406524));
#35067=CARTESIAN_POINT('Ctrl Pts',(-0.186874209749804,0.0700626557706258,
-0.760670974369452));
#35068=CARTESIAN_POINT('Ctrl Pts',(-0.160171076857274,-0.119062891539001,
-0.749553191332379));
#35069=CARTESIAN_POINT('Ctrl Pts',(0.0132349557812702,-0.199137093352079,
-0.738435408295307));
#35070=CARTESIAN_POINT('Ctrl Pts',(0.174518909769793,-0.0968188831582442,
-0.727317625258234));
#35071=CARTESIAN_POINT('Ctrl Pts',(0.175958585839427,0.0941770782761695,
-0.716199842221161));
#35072=CARTESIAN_POINT('Ctrl Pts',(0.0162353648096416,0.198914954019915,
-0.70508205918409));
#35073=CARTESIAN_POINT('Ctrl Pts',(-0.158358050906612,0.121463878236724,
-0.693964276147017));
#35074=CARTESIAN_POINT('Ctrl Pts',(-0.187909142365856,-0.0672376398944485,
-0.682846493109945));
#35075=CARTESIAN_POINT('Ctrl Pts',(-0.0453516570786103,-0.194355275728422,
-0.671728710072871));
#35076=CARTESIAN_POINT('Ctrl Pts',(0.138744036805732,-0.143460232308806,
-0.660610927035801));
#35077=CARTESIAN_POINT('Ctrl Pts',(0.195762152632669,0.0388320177156751,
-0.649493143998727));
#35078=CARTESIAN_POINT('Ctrl Pts',(0.0734790112337116,0.185557486810322,
-0.638375360961656));
#35079=CARTESIAN_POINT('Ctrl Pts',(-0.116104570606568,0.162328292935986,
-0.627257577924582));
#35080=CARTESIAN_POINT('Ctrl Pts',(-0.199346373918836,-0.00957962466167244,
-0.616139794887511));
#35081=CARTESIAN_POINT('Ctrl Pts',(-0.100004082264906,-0.172713431827408,
-0.605022011850438));
#35082=CARTESIAN_POINT('Ctrl Pts',(0.0909333284489641,-0.177656623238313,
-0.593904228813366));
#35083=CARTESIAN_POINT('Ctrl Pts',(0.198583648704504,-0.01988166166227,
-0.582786445776293));
#35084=CARTESIAN_POINT('Ctrl Pts',(0.124348464543696,0.156103188208544,
-0.571668662739221));
#35085=CARTESIAN_POINT('Ctrl Pts',(-0.0637791943725893,0.189110973685903,
-0.560550879702148));
#35086=CARTESIAN_POINT('Ctrl Pts',(-0.193490608973672,0.0489094085247839,
-0.549433096665077));
#35087=CARTESIAN_POINT('Ctrl Pts',(-0.145981304534738,-0.136088958881986,
-0.538315313628003));
#35088=CARTESIAN_POINT('Ctrl Pts',(0.0352342913530302,-0.196441570743304,
-0.527197530590931));
#35089=CARTESIAN_POINT('Ctrl Pts',(0.184178313537193,-0.0768706369548383,
-0.516079747553859));
#35090=CARTESIAN_POINT('Ctrl Pts',(0.164430876586609,0.113107174079306,
-0.504961964516787));
#35091=CARTESIAN_POINT('Ctrl Pts',(-0.00592106946976007,0.199488563430541,
-0.493844181479714));
#35092=CARTESIAN_POINT('Ctrl Pts',(-0.170849826284632,0.103155624479512,
-0.482726398442642));
#35093=CARTESIAN_POINT('Ctrl Pts',(-0.179294869380122,-0.087658974538901,
-0.471608615405569));
#35094=CARTESIAN_POINT('Ctrl Pts',(-0.0235212672386517,-0.198185509033164,
-0.460490832368497));
#35095=CARTESIAN_POINT('Ctrl Pts',(0.15379578817364,-0.127191200730621,
-0.449373049331425));
#35096=CARTESIAN_POINT('Ctrl Pts',(0.190249158727879,0.0602992836323975,
-0.438255266294352));
#35097=CARTESIAN_POINT('Ctrl Pts',(0.052450699256103,0.192560821951897,
-0.42713748325728));
#35098=CARTESIAN_POINT('Ctrl Pts',(-0.133388079514004,0.148453245996245,
-0.416019700220208));
#35099=CARTESIAN_POINT('Ctrl Pts',(-0.197054875425419,-0.0316247067070998,
-0.404901917183135));
#35100=CARTESIAN_POINT('Ctrl Pts',(-0.0802363914648483,-0.182737154098266,
-0.393784134146063));
#35101=CARTESIAN_POINT('Ctrl Pts',(0.110071710746651,-0.166478120173837,
-0.38266635110899));
#35102=CARTESIAN_POINT('Ctrl Pts',(0.199563614032374,0.00226052151145618,
-0.371548568071918));
#35103=CARTESIAN_POINT('Ctrl Pts',(0.106272449134592,0.168928720347144,
-0.360430785034846));
#35104=CARTESIAN_POINT('Ctrl Pts',(-0.0843551185474909,0.18087277290543,
-0.349313001997773));
#35105=CARTESIAN_POINT('Ctrl Pts',(-0.197720669000457,0.0271529566091497,
-0.338195218960701));
#35106=CARTESIAN_POINT('Ctrl Pts',(-0.129991130062581,-0.151436627366443,
-0.327077435923628));
#35107=CARTESIAN_POINT('Ctrl Pts',(0.056799078860964,-0.191323314435221,
-0.315959652886556));
#35108=CARTESIAN_POINT('Ctrl Pts',(0.191566227578033,-0.055974337422329,
-0.304841869849484));
#35109=CARTESIAN_POINT('Ctrl Pts',(0.150875224767089,0.130642307676758,
-0.293724086812411));
#35110=CARTESIAN_POINT('Ctrl Pts',(-0.0280044786374454,0.197601860306157,
-0.282606303775339));
#35111=CARTESIAN_POINT('Ctrl Pts',(-0.181234493456315,0.0835751419292736,
-0.271488520738266));
#35112=CARTESIAN_POINT('Ctrl Pts',(-0.168469334814571,-0.106999202071807,
-0.260370737701194));
#35113=CARTESIAN_POINT('Ctrl Pts',(-0.00140078699449221,-0.199571500727773,
-0.249252954664122));
#35114=CARTESIAN_POINT('Ctrl Pts',(0.166950760111813,-0.109353506747779,
-0.238135171627049));
#35115=CARTESIAN_POINT('Ctrl Pts',(0.182389803640612,0.0810228714550746,
-0.227017388589977));
#35116=CARTESIAN_POINT('Ctrl Pts',(0.0307755058387974,0.197189286857941,
-0.215899605552904));
#35117=CARTESIAN_POINT('Ctrl Pts',(-0.149026496594129,0.132747306769101,
-0.204781822515832));
#35118=CARTESIAN_POINT('Ctrl Pts',(-0.192333085348998,-0.0532797515233865,
-0.19366403947876));
#35119=CARTESIAN_POINT('Ctrl Pts',(-0.0594791256025773,-0.190507173048921,
-0.182546256441687));
#35120=CARTESIAN_POINT('Ctrl Pts',(0.127852545543535,-0.153246402000575,
-0.171428473404615));
#35121=CARTESIAN_POINT('Ctrl Pts',(0.198082383035612,0.0243747804091565,
-0.160310690367542));
#35122=CARTESIAN_POINT('Ctrl Pts',(0.0868856852284144,0.179670923258195,
-0.14919290733047));
#35123=CARTESIAN_POINT('Ctrl Pts',(-0.103890530912397,0.170403686824479,
-0.138075124293398));
#35124=CARTESIAN_POINT('Ctrl Pts',(-0.199512508665682,0.00506193506719449,
-0.126957341256325));
#35125=CARTESIAN_POINT('Ctrl Pts',(-0.112397212591169,-0.164917203682897,
-0.115839558219253));
#35126=CARTESIAN_POINT('Ctrl Pts',(0.0776623121413626,-0.183844323471358,
-0.10472177518218));
#35127=CARTESIAN_POINT('Ctrl Pts',(0.196593525860617,-0.034389841833708,
-0.0936039921451079));
#35128=CARTESIAN_POINT('Ctrl Pts',(0.135455026238565,0.146570291745065,
-0.0824862091080354));
#35129=CARTESIAN_POINT('Ctrl Pts',(-0.049735296985837,0.19327035668827,
-0.0713684260709631));
#35130=CARTESIAN_POINT('Ctrl Pts',(-0.18939769988277,0.0629786854978793,
-0.0602506430338908));
#35131=CARTESIAN_POINT('Ctrl Pts',(-0.155539915651925,-0.125047929923611,
-0.0491328599968184));
#35132=CARTESIAN_POINT('Ctrl Pts',(0.0206870796054742,-0.198442384758988,
-0.0380150769597463));
#35133=CARTESIAN_POINT('Ctrl Pts',(0.178142926080333,-0.0902714528615779,
-0.0268972939226737));
#35134=CARTESIAN_POINT('Ctrl Pts',(0.172087026372346,0.100962540838038,
-0.0157795108856014));
#35135=CARTESIAN_POINT('Ctrl Pts',(0.0634850318392476,0.166218031662509,
-0.00836765552755316));
#35136=CARTESIAN_POINT('Ctrl Pts',(0.00737739821677115,0.168672073681436,
-0.00466172784852903));
#35137=CARTESIAN_POINT('Ctrl Pts',(0.0903606778650232,-0.126612599672282,
-1.5646));
#35138=CARTESIAN_POINT('Ctrl Pts',(0.132477509652,-0.0965547264460079,-1.56089407232098));
#35139=CARTESIAN_POINT('Ctrl Pts',(0.183629629053462,0.00837163889085661,
-1.55348221696293));
#35140=CARTESIAN_POINT('Ctrl Pts',(0.0923230570238932,0.159158029769189,
-1.54236443392586));
#35141=CARTESIAN_POINT('Ctrl Pts',(-0.0836206488085049,0.163699342626539,
-1.53124665088878));
#35142=CARTESIAN_POINT('Ctrl Pts',(-0.182934470289723,0.0185420837280834,
-1.52012886785171));
#35143=CARTESIAN_POINT('Ctrl Pts',(-0.114717412999509,-0.14372078954814,
-1.50901108481464));
#35144=CARTESIAN_POINT('Ctrl Pts',(0.0585821121664253,-0.174283509875506,
-1.49789330177756));
#35145=CARTESIAN_POINT('Ctrl Pts',(0.178219584548083,-0.0452513232337437,
-1.4867755187405));
#35146=CARTESIAN_POINT('Ctrl Pts',(0.134626373349144,0.125244912864161,
-1.47565773570342));
#35147=CARTESIAN_POINT('Ctrl Pts',(-0.0322746164076941,0.18101828554357,
-1.46453995266635));
#35148=CARTESIAN_POINT('Ctrl Pts',(-0.169613985667002,0.0709994086342611,
-1.45342216962927));
#35149=CARTESIAN_POINT('Ctrl Pts',(-0.151602013332166,-0.104051378974232,
-1.4423043865922));
#35150=CARTESIAN_POINT('Ctrl Pts',(0.00526457092671344,-0.183798721027812,
-1.43118660355513));
#35151=CARTESIAN_POINT('Ctrl Pts',(0.157309138173746,-0.095202988083288,
-1.42006882051806));
#35152=CARTESIAN_POINT('Ctrl Pts',(0.165272159879762,0.0805908485969487,
-1.40895103748099));
#35153=CARTESIAN_POINT('Ctrl Pts',(0.021860095314849,0.182570218824516,
-1.39783325444391));
#35154=CARTESIAN_POINT('Ctrl Pts',(-0.141573914269114,0.117331109047258,
-1.38671547140684));
#35155=CARTESIAN_POINT('Ctrl Pts',(-0.17533843141003,-0.0553732368534328,
-1.37559768836977));
#35156=CARTESIAN_POINT('Ctrl Pts',(-0.048508054493723,-0.177360442508133,
-1.3644799053327));
#35157=CARTESIAN_POINT('Ctrl Pts',(0.12275151636726,-0.136900786130964,
-1.35336212229563));
#35158=CARTESIAN_POINT('Ctrl Pts',(0.181581280715027,0.0289481974204555,
-1.34224433925855));
#35159=CARTESIAN_POINT('Ctrl Pts',(0.0740982434113141,0.1682831233296,-1.33112655622148));
#35160=CARTESIAN_POINT('Ctrl Pts',(-0.101252397253136,0.153485216344168,
-1.32000877318441));
#35161=CARTESIAN_POINT('Ctrl Pts',(-0.183864570130966,-0.00189191961280822,
-1.30889099014733));
#35162=CARTESIAN_POINT('Ctrl Pts',(-0.0980726456853608,-0.155536219688844,
-1.29777320711026));
#35163=CARTESIAN_POINT('Ctrl Pts',(0.0775453683472552,-0.166722749977294,
-1.28665542407319));
#35164=CARTESIAN_POINT('Ctrl Pts',(0.18213850936899,-0.025205612527195,
-1.27553764103612));
#35165=CARTESIAN_POINT('Ctrl Pts',(0.119908476028974,0.139397693201698,
-1.26441985799905));
#35166=CARTESIAN_POINT('Ctrl Pts',(-0.0521473853035587,0.176324728004856,
-1.25330207496197));
#35167=CARTESIAN_POINT('Ctrl Pts',(-0.176440736777005,0.0517535110223655,
-1.2421842919249));
#35168=CARTESIAN_POINT('Ctrl Pts',(-0.139129582451151,-0.120219460920973,
-1.23106650888783));
#35169=CARTESIAN_POINT('Ctrl Pts',(0.0256122765083437,-0.182081769516105,
-1.21994872585076));
#35170=CARTESIAN_POINT('Ctrl Pts',(0.166895497950393,-0.0771728725754398,
-1.20883094281368));
#35171=CARTESIAN_POINT('Ctrl Pts',(0.155316829566065,0.0984197233850115,
-1.19771315977661));
#35172=CARTESIAN_POINT('Ctrl Pts',(0.00148133352129465,0.183868336449635,
-1.18659537673954));
#35173=CARTESIAN_POINT('Ctrl Pts',(-0.153710936338967,0.100909402671365,
-1.17547759370247));
#35174=CARTESIAN_POINT('Ctrl Pts',(-0.168117238307517,-0.0744738456207954,
-1.16435981066539));
#35175=CARTESIAN_POINT('Ctrl Pts',(-0.0285426415962272,-0.181645470927358,
-1.15324202762832));
#35176=CARTESIAN_POINT('Ctrl Pts',(0.137174554457832,-0.122445502600127,
-1.14212424459125));
#35177=CARTESIAN_POINT('Ctrl Pts',(0.177251682996677,0.0489039913764663,
-1.13100646155418));
#35178=CARTESIAN_POINT('Ctrl Pts',(0.0549815489042986,0.175461644748333,
-1.11988867851711));
#35179=CARTESIAN_POINT('Ctrl Pts',(-0.117646944606339,0.141311556224172,
-1.10877089548003));
#35180=CARTESIAN_POINT('Ctrl Pts',(-0.182520977956929,-0.0222677368259724,
-1.09765311244296));
#35181=CARTESIAN_POINT('Ctrl Pts',(-0.0802215287029169,-0.165451702409712,
-1.08653532940589));
#35182=CARTESIAN_POINT('Ctrl Pts',(0.0955539257930597,-0.157096170428305,
-1.07541754636882));
#35183=CARTESIAN_POINT('Ctrl Pts',(0.183810220956364,-0.00485408793464279,
-1.06429976333174));
#35184=CARTESIAN_POINT('Ctrl Pts',(0.103712198059592,0.151833920687547,
-1.05318198029467));
#35185=CARTESIAN_POINT('Ctrl Pts',(-0.0713772583275903,0.169455145957098,
-1.0420641972576));
#35186=CARTESIAN_POINT('Ctrl Pts',(-0.181091298765559,0.031870064466641,
-1.03094641422053));
#35187=CARTESIAN_POINT('Ctrl Pts',(-0.12494131950069,-0.134905248893923,
-1.01982863118345));
#35188=CARTESIAN_POINT('Ctrl Pts',(0.0456441385565052,-0.178118983022976,
-1.00871084814638));
#35189=CARTESIAN_POINT('Ctrl Pts',(0.174423500194588,-0.0581910824574806,
-0.997593065109308));
#35190=CARTESIAN_POINT('Ctrl Pts',(0.143445970860419,0.11503483360103,-0.986475282072236));
#35191=CARTESIAN_POINT('Ctrl Pts',(-0.0189157028212204,0.182898758017883,
-0.975357499035165));
#35192=CARTESIAN_POINT('Ctrl Pts',(-0.163952223241389,0.0832431858587246,
-0.96423971599809));
#35193=CARTESIAN_POINT('Ctrl Pts',(-0.158822639760351,-0.0926559690319977,
-0.95312193296102));
#35194=CARTESIAN_POINT('Ctrl Pts',(-0.00822520867957112,-0.183690243180965,
-0.942004149923946));
#35195=CARTESIAN_POINT('Ctrl Pts',(0.14990580454341,-0.106480088570106,
-0.930886366886874));
#35196=CARTESIAN_POINT('Ctrl Pts',(0.170736022599271,0.0682566486482162,
-0.919768583849802));
#35197=CARTESIAN_POINT('Ctrl Pts',(0.0351867613017287,0.18047617938886,
-0.908650800812729));
#35198=CARTESIAN_POINT('Ctrl Pts',(-0.132590540269491,0.127395086752784,
-0.897533017775657));
#35199=CARTESIAN_POINT('Ctrl Pts',(-0.178926336182619,-0.0423689239652017,
-0.886415234738584));
#35200=CARTESIAN_POINT('Ctrl Pts',(-0.0613810315003473,-0.173326652508083,
-0.875297451701512));
#35201=CARTESIAN_POINT('Ctrl Pts',(0.112384007026421,-0.145532108011909,
-0.86417966866444));
#35202=CARTESIAN_POINT('Ctrl Pts',(0.183214982554139,0.0155573026386719,
-0.853061885627367));
#35203=CARTESIAN_POINT('Ctrl Pts',(0.086236827089008,0.162397565102822,
-0.841944102590294));
#35204=CARTESIAN_POINT('Ctrl Pts',(-0.0897268284244655,0.160495656510048,
-0.830826319553223));
#35205=CARTESIAN_POINT('Ctrl Pts',(-0.183508443502437,0.0115935611878976,
-0.819708536516149));
#35206=CARTESIAN_POINT('Ctrl Pts',(-0.109212142655086,-0.14792723682402,
-0.808590753479079));
#35207=CARTESIAN_POINT('Ctrl Pts',(0.0651130668400682,-0.171959437148373,
-0.797472970442005));
#35208=CARTESIAN_POINT('Ctrl Pts',(0.179800319818854,-0.0384916158499819,
-0.786355187404933));
#35209=CARTESIAN_POINT('Ctrl Pts',(0.129805978528337,0.130231207611715,
-0.775237404367861));
#35210=CARTESIAN_POINT('Ctrl Pts',(-0.039079449893004,0.179673470756717,
-0.764119621330788));
#35211=CARTESIAN_POINT('Ctrl Pts',(-0.172171470838591,0.0645503224390171,
-0.753001838293716));
#35212=CARTESIAN_POINT('Ctrl Pts',(-0.147569265578375,-0.109695357031935,
-0.741884055256643));
#35213=CARTESIAN_POINT('Ctrl Pts',(0.0121936665653112,-0.183469545138692,
-0.730766272219571));
#35214=CARTESIAN_POINT('Ctrl Pts',(0.160788251222258,-0.0892014448683006,
-0.719648489182499));
#35215=CARTESIAN_POINT('Ctrl Pts',(0.162114657614943,0.0867674897879067,
-0.708530706145426));
#35216=CARTESIAN_POINT('Ctrl Pts',(0.014958011823137,0.183264883106403,
-0.697412923108354));
#35217=CARTESIAN_POINT('Ctrl Pts',(-0.145898883426596,0.111907440827576,
-0.686295140071281));
#35218=CARTESIAN_POINT('Ctrl Pts',(-0.1731249778579,-0.0619475708918949,
-0.675177357034209));
#35219=CARTESIAN_POINT('Ctrl Pts',(-0.041783515845475,-0.179063947519582,
-0.664059573997137));
#35220=CARTESIAN_POINT('Ctrl Pts',(0.127828044966229,-0.132173183429228,
-0.652941790960064));
#35221=CARTESIAN_POINT('Ctrl Pts',(0.180360135293257,0.0357768234294574,
-0.641824007922992));
#35222=CARTESIAN_POINT('Ctrl Pts',(0.0676978886322038,0.170958343968484,
-0.630706224885919));
#35223=CARTESIAN_POINT('Ctrl Pts',(-0.106969788496654,0.149556757943885,
-0.619588441848848));
#35224=CARTESIAN_POINT('Ctrl Pts',(-0.183662360097186,-0.00882592665028588,
-0.608470658811774));
#35225=CARTESIAN_POINT('Ctrl Pts',(-0.0921360414391275,-0.159124823222627,
-0.597352875774703));
#35226=CARTESIAN_POINT('Ctrl Pts',(0.0837789491030789,-0.163679098191823,
-0.58623509273763));
#35227=CARTESIAN_POINT('Ctrl Pts',(0.182959643964377,-0.01831742826199,
-0.575117309700558));
#35228=CARTESIAN_POINT('Ctrl Pts',(0.114565075971008,0.143821427003983,
-0.563999526663485));
#35229=CARTESIAN_POINT('Ctrl Pts',(-0.0587612261677574,0.174232252459085,
-0.552881743626413));
#35230=CARTESIAN_POINT('Ctrl Pts',(-0.178267310320956,0.0450613533822114,
-0.54176396058934));
#35231=CARTESIAN_POINT('Ctrl Pts',(-0.134495904760386,-0.12538186112987,
-0.530646177552268));
#35232=CARTESIAN_POINT('Ctrl Pts',(0.032462156090606,-0.180986098691733,
-0.519528394515196));
#35233=CARTESIAN_POINT('Ctrl Pts',(0.169687680181897,-0.0708226707501974,
-0.508410611478123));
#35234=CARTESIAN_POINT('Ctrl Pts',(0.151493916207583,0.104208218724794,
-0.497292828441051));
#35235=CARTESIAN_POINT('Ctrl Pts',(-0.00545521632391679,0.183793362536746,
-0.486175045403978));
#35236=CARTESIAN_POINT('Ctrl Pts',(-0.157407840939238,0.0950396291478065,
-0.475057262366907));
#35237=CARTESIAN_POINT('Ctrl Pts',(-0.165188451720106,-0.0807622121788323,
-0.463939479329833));
#35238=CARTESIAN_POINT('Ctrl Pts',(-0.0216706798754521,-0.182592828806171,
-0.452821696292762));
#35239=CARTESIAN_POINT('Ctrl Pts',(0.141695566734905,-0.117184153644509,
-0.441703913255688));
#35240=CARTESIAN_POINT('Ctrl Pts',(0.175280888292921,0.0555551050484869,
-0.430586130218617));
#35241=CARTESIAN_POINT('Ctrl Pts',(0.0483240252869895,0.177410676335346,
-0.419468347181544));
#35242=CARTESIAN_POINT('Ctrl Pts',(-0.1228934793785,0.136773360797922,-0.408350564144472));
#35243=CARTESIAN_POINT('Ctrl Pts',(-0.181551150280891,-0.0291365634449526,
-0.397232781107399));
#35244=CARTESIAN_POINT('Ctrl Pts',(-0.0739236171314337,-0.168359907127257,
-0.386114998070327));
#35245=CARTESIAN_POINT('Ctrl Pts',(0.101411577137068,-0.153380088408926,
-0.374997215033255));
#35246=CARTESIAN_POINT('Ctrl Pts',(0.183862508367636,0.00208267001642915,
-0.363879431996182));
#35247=CARTESIAN_POINT('Ctrl Pts',(0.0979112307772101,0.155637882230987,
-0.35276164895911));
#35248=CARTESIAN_POINT('Ctrl Pts',(-0.0777182943142881,0.166642210219781,
-0.341643865922037));
#35249=CARTESIAN_POINT('Ctrl Pts',(-0.182164561084034,0.025016638107916,
-0.330526082884965));
#35250=CARTESIAN_POINT('Ctrl Pts',(-0.119763792386384,-0.139522018085984,
-0.319408299847893));
#35251=CARTESIAN_POINT('Ctrl Pts',(0.0523302865754574,-0.176270532440662,
-0.30829051681082));
#35252=CARTESIAN_POINT('Ctrl Pts',(0.176494333858419,-0.0515704334810062,
-0.297172733773748));
#35253=CARTESIAN_POINT('Ctrl Pts',(0.139004785069224,0.12036373717149,-0.286054950736676));
#35254=CARTESIAN_POINT('Ctrl Pts',(-0.0258011647703144,0.182055099924714,
-0.274937167699603));
#35255=CARTESIAN_POINT('Ctrl Pts',(-0.166975471611825,0.0769996840696845,
-0.26381938466253));
#35256=CARTESIAN_POINT('Ctrl Pts',(-0.155214639864204,-0.0985808048308175,
-0.252701601625459));
#35257=CARTESIAN_POINT('Ctrl Pts',(-0.0012905770009465,-0.183869774559952,
-0.241583818588386));
#35258=CARTESIAN_POINT('Ctrl Pts',(0.153815542361654,-0.100749879415303,
-0.230466035551314));
#35259=CARTESIAN_POINT('Ctrl Pts',(0.168039885229795,0.0746482190809691,
-0.219348252514241));
#35260=CARTESIAN_POINT('Ctrl Pts',(0.0283541753201865,0.181674986598733,
-0.208230469477169));
#35261=CARTESIAN_POINT('Ctrl Pts',(-0.137301509645904,0.122303120836724,
-0.197112686440096));
#35262=CARTESIAN_POINT('Ctrl Pts',(-0.177200857409891,-0.0490878500461769,
-0.185994903403024));
#35263=CARTESIAN_POINT('Ctrl Pts',(-0.0547994747530945,-0.175518602770541,
-0.174877120365952));
#35264=CARTESIAN_POINT('Ctrl Pts',(0.11779346570166,-0.141189404725702,
-0.163759337328879));
#35265=CARTESIAN_POINT('Ctrl Pts',(0.182497816472988,0.0224570410225731,
-0.152641554291807));
#35266=CARTESIAN_POINT('Ctrl Pts',(0.080049763103335,0.16553491873334,-0.141523771254734));
#35267=CARTESIAN_POINT('Ctrl Pts',(-0.0957167152029026,0.156996802481032,
-0.130405988217662));
#35268=CARTESIAN_POINT('Ctrl Pts',(-0.183815423827918,0.00466367620751416,
-0.11928820518059));
#35269=CARTESIAN_POINT('Ctrl Pts',(-0.103554115016128,-0.15194198045138,
-0.108170422143517));
#35270=CARTESIAN_POINT('Ctrl Pts',(0.0715520591525512,-0.169379967518084,
-0.0970526391064447));
#35271=CARTESIAN_POINT('Ctrl Pts',(0.181126098406431,-0.0316841454920027,
-0.0859348560693724));
#35272=CARTESIAN_POINT('Ctrl Pts',(0.124797804529567,0.135038552108262,
-0.0748170730322999));
#35273=CARTESIAN_POINT('Ctrl Pts',(-0.0458222632545728,0.17806438686788,
-0.0636992899952276));
#35274=CARTESIAN_POINT('Ctrl Pts',(-0.174496419842635,0.0580236990870384,
-0.0525815069581552));
#35275=CARTESIAN_POINT('Ctrl Pts',(-0.143302471152953,-0.115209509375821,
-0.0414637239210829));
#35276=CARTESIAN_POINT('Ctrl Pts',(0.0190594781794568,-0.182829494270053,
-0.0303459408840108));
#35277=CARTESIAN_POINT('Ctrl Pts',(0.16412714008961,-0.083169148031303,
-0.0192281578469382));
#35278=CARTESIAN_POINT('Ctrl Pts',(0.158547701592606,0.0930190911788169,
-0.00811037480986587));
#35279=CARTESIAN_POINT('Ctrl Pts',(0.0584902075178373,0.153140462932497,
-0.000698519451817671));
#35280=CARTESIAN_POINT('Ctrl Pts',(0.0067969652080078,0.155401427805413,
0.00300740822720647));
#35281=CARTESIAN_POINT('Ctrl Pts',(0.00853826423430342,0.195213365433479,
-0.0200000000000003));
#35282=CARTESIAN_POINT('Ctrl Pts',(0.0734746804820721,0.19237316912253,
-0.0237059276790243));
#35283=CARTESIAN_POINT('Ctrl Pts',(0.136320178206947,0.154611304639505,
-0.0274118553580483));
#35284=CARTESIAN_POINT('Ctrl Pts',(0.168911064091045,0.0988427886182253,
-0.0311177830370723));
#35285=CARTESIAN_POINT('Ctrl Pts',(0.201501949975142,0.0430742725969455,
-0.0348237107160964));
#35286=CARTESIAN_POINT('Ctrl Pts',(0.203838224018461,-0.0307008949625867,
-0.0385296383951203));
#35287=CARTESIAN_POINT('Ctrl Pts',(0.174634325106077,-0.0884538292781432,
-0.0422355660741444));
#35288=CARTESIAN_POINT('Ctrl Pts',(0.145430426193693,-0.146206763593701,
-0.0459414937531686));
#35289=CARTESIAN_POINT('Ctrl Pts',(0.0846863543255994,-0.187937464665282,
-0.049647421432193));
#35290=CARTESIAN_POINT('Ctrl Pts',(0.0203214705403238,-0.194645582748126,
-0.0533533491112172));
#35291=CARTESIAN_POINT('Ctrl Pts',(-0.0440434132449519,-0.20135370083097,
-0.0570592767902414));
#35292=CARTESIAN_POINT('Ctrl Pts',(-0.112029108947411,-0.17303923592508,
-0.0607652044692654));
#35293=CARTESIAN_POINT('Ctrl Pts',(-0.152552866017503,-0.122613098582343,
-0.0644711321482895));
#35294=CARTESIAN_POINT('Ctrl Pts',(-0.180042705249534,-0.0884058456307822,
-0.0669850983613853));
#35295=CARTESIAN_POINT('Ctrl Pts',(-0.194895189472664,-0.0440233075995439,
-0.069499064574481));
#35296=CARTESIAN_POINT('Ctrl Pts',(-0.195234571671998,0.00015548015543182,
-0.0720130307875768));
#35297=CARTESIAN_POINT('Origin',(0.,0.,-0.02));
#35298=CARTESIAN_POINT('',(-0.2154,2.6378892053634E-17,0.));
#35299=CARTESIAN_POINT('Origin',(-0.2154,-2.6378892053634E-17,-0.02));
#35300=CARTESIAN_POINT('Origin',(0.,0.,0.));
#35301=CARTESIAN_POINT('Origin',(0.,0.,-0.02));
#35302=CARTESIAN_POINT('Origin',(0.,0.,-0.78));
#35303=CARTESIAN_POINT('Origin',(0.35,0.,0.));
#35304=CARTESIAN_POINT('',(0.330485534147499,-0.115235895966675,0.));
#35305=CARTESIAN_POINT('',(0.317616105825637,-0.115602808444076,0.));
#35306=CARTESIAN_POINT('',(0.335441504501922,-0.115094599297143,0.));
#35307=CARTESIAN_POINT('',(0.327238813083405,-0.124156188777542,0.));
#35308=CARTESIAN_POINT('',(0.318650451154949,-0.116522211763823,0.));
#35309=CARTESIAN_POINT('',(0.305454212950408,-0.170873414523286,0.));
#35310=CARTESIAN_POINT('Origin',(0.,0.,0.));
#35311=CARTESIAN_POINT('',(0.29271658647914,-0.169,0.));
#35312=CARTESIAN_POINT('',(0.308586965898532,-0.171334171076645,-2.77555756156289E-17));
#35313=CARTESIAN_POINT('',(0.300707824283758,-0.179094400846393,0.));
#35314=CARTESIAN_POINT('',(0.279811089486919,-0.152697987352333,0.));
#35315=CARTESIAN_POINT('',(0.27114182006011,-0.221319030845725,0.));
#35316=CARTESIAN_POINT('Origin',(0.,0.,0.));
#35317=CARTESIAN_POINT('',(0.258923021774215,-0.21726221207405,0.));
#35318=CARTESIAN_POINT('',(0.267454002283238,-0.22009462169896,-2.77555756156289E-17));
#35319=CARTESIAN_POINT('',(0.265039980408751,-0.228590920171666,0.));
#35320=CARTESIAN_POINT('',(0.236940191931664,-0.176549649291667,5.55111512312578E-17));
#35321=CARTESIAN_POINT('',(0.228590920171666,-0.265039980408751,0.));
#35322=CARTESIAN_POINT('Origin',(0.,0.,0.));
#35323=CARTESIAN_POINT('',(0.21726221207405,-0.258923021774215,0.));
#35324=CARTESIAN_POINT('',(0.214525877254124,-0.257445532305909,0.));
#35325=CARTESIAN_POINT('',(0.221319030845725,-0.27114182006011,0.));
#35326=CARTESIAN_POINT('',(0.193859348761916,-0.188435558020616,-2.77555756156289E-17));
#35327=CARTESIAN_POINT('',(0.179094400846393,-0.300707824283758,0.));
#35328=CARTESIAN_POINT('Origin',(0.,0.,0.));
#35329=CARTESIAN_POINT('',(0.169,-0.29271658647914,0.));
#35330=CARTESIAN_POINT('',(0.153407416225873,-0.280372709232379,0.));
#35331=CARTESIAN_POINT('',(0.170873414523285,-0.305454212950408,0.));
#35332=CARTESIAN_POINT('',(0.153874180716026,-0.189873871363808,0.));
#35333=CARTESIAN_POINT('',(0.124156188777542,-0.327238813083405,0.));
#35334=CARTESIAN_POINT('Origin',(0.,0.,0.));
#35335=CARTESIAN_POINT('',(0.115602808444076,-0.317616105825637,0.));
#35336=CARTESIAN_POINT('',(0.0884746524536336,-0.287096440691874,0.));
#35337=CARTESIAN_POINT('',(0.115235895966675,-0.330485534147499,0.));
#35338=CARTESIAN_POINT('',(0.119433076204517,-0.183269744138128,2.77555756156289E-17));
#35339=CARTESIAN_POINT('',(0.0654455537387477,-0.343826816138341,0.));
#35340=CARTESIAN_POINT('Origin',(0.,0.,0.));
#35341=CARTESIAN_POINT('',(0.0586930840514223,-0.332865020518126,0.));
#35342=CARTESIAN_POINT('',(0.0244380373436002,-0.277256207985893,2.77555756156289E-17));
#35343=CARTESIAN_POINT('',(0.0560969930232948,-0.345475219623267,0.));
#35344=CARTESIAN_POINT('',(0.0919040248701096,-0.171546880416256,0.));
#35345=CARTESIAN_POINT('',(0.00474638866665021,-0.349967815369678,0.));
#35346=CARTESIAN_POINT('Origin',(0.,0.,0.));
#35347=CARTESIAN_POINT('',(-6.20895927167708E-17,-0.338,0.));
#35348=CARTESIAN_POINT('',(-0.0341308674003153,-0.251940482303103,-2.77555756156289E-17));
#35349=CARTESIAN_POINT('',(-0.00474638866665032,-0.349967815369678,0.));
#35350=CARTESIAN_POINT('',(0.0714942725679436,-0.157730259324412,0.));
#35351=CARTESIAN_POINT('',(-0.0560969930232949,-0.345475219623267,0.));
#35352=CARTESIAN_POINT('Origin',(0.,0.,0.));
#35353=CARTESIAN_POINT('',(-0.0586930840514224,-0.332865020518126,0.));
#35354=CARTESIAN_POINT('',(-0.0832550096107083,-0.213558429049481,0.));
#35355=CARTESIAN_POINT('',(-0.0654455537387478,-0.343826816138341,0.));
#35356=CARTESIAN_POINT('',(0.0573199163702635,-0.144532327622448,5.55111512312578E-17));
#35357=CARTESIAN_POINT('',(-0.115235895966675,-0.330485534147499,0.));
#35358=CARTESIAN_POINT('Origin',(0.,0.,0.));
#35359=CARTESIAN_POINT('',(-0.115602808444076,-0.317616105825637,0.));
#35360=CARTESIAN_POINT('',(-0.11993773416091,-0.1655689032104,0.));
#35361=CARTESIAN_POINT('',(-0.124156188777542,-0.327238813083405,0.));
#35362=CARTESIAN_POINT('',(0.0476141712835098,-0.13399405767813,0.));
#35363=CARTESIAN_POINT('',(-0.170873414523286,-0.305454212950408,0.));
#35364=CARTESIAN_POINT('Origin',(0.,0.,0.));
#35365=CARTESIAN_POINT('',(-0.169,-0.29271658647914,0.));
#35366=CARTESIAN_POINT('',(-0.142435244588531,-0.112098828088702,0.));
#35367=CARTESIAN_POINT('',(-0.179094400846393,-0.300707824283758,0.));
#35368=CARTESIAN_POINT('',(0.0400460999029137,-0.127225130188389,0.));
#35369=CARTESIAN_POINT('',(-0.221319030845725,-0.27114182006011,0.));
#35370=CARTESIAN_POINT('Origin',(0.,0.,0.));
#35371=CARTESIAN_POINT('',(-0.21726221207405,-0.258923021774215,0.));
#35372=CARTESIAN_POINT('',(-0.150385479533696,-0.0574959058685693,0.));
#35373=CARTESIAN_POINT('',(-0.228590920171666,-0.265039980408751,0.));
#35374=CARTESIAN_POINT('',(0.0321081520112096,-0.124274994069283,0.));
#35375=CARTESIAN_POINT('',(-0.265039980408751,-0.228590920171666,0.));
#35376=CARTESIAN_POINT('Origin',(0.,0.,0.));
#35377=CARTESIAN_POINT('',(-0.258923021774215,-0.21726221207405,0.));
#35378=CARTESIAN_POINT('',(-0.144780334443528,-0.00586807595124715,0.));
#35379=CARTESIAN_POINT('',(-0.27114182006011,-0.221319030845725,0.));
#35380=CARTESIAN_POINT('',(0.0215225383940517,-0.124150206596651,0.));
#35381=CARTESIAN_POINT('',(-0.300707824283758,-0.179094400846393,0.));
#35382=CARTESIAN_POINT('Origin',(0.,0.,0.));
#35383=CARTESIAN_POINT('',(-0.29271658647914,-0.169,0.));
#35384=CARTESIAN_POINT('',(-0.127786749933849,0.0393366710293742,0.));
#35385=CARTESIAN_POINT('',(-0.305454212950408,-0.170873414523285,0.));
#35386=CARTESIAN_POINT('',(0.00661426644602217,-0.124975254227913,-2.77555756156289E-17));
#35387=CARTESIAN_POINT('',(-0.327238813083405,-0.124156188777542,0.));
#35388=CARTESIAN_POINT('Origin',(0.,0.,0.));
#35389=CARTESIAN_POINT('',(-0.317616105825637,-0.115602808444076,0.));
#35390=CARTESIAN_POINT('',(-0.102440047215055,0.0756617305936987,0.));
#35391=CARTESIAN_POINT('',(-0.330485534147499,-0.115235895966675,0.));
#35392=CARTESIAN_POINT('',(-0.0133971428466065,-0.124276211068284,-2.77555756156289E-17));
#35393=CARTESIAN_POINT('',(-0.343826816138341,-0.0654455537387478,0.));
#35394=CARTESIAN_POINT('Origin',(0.,0.,0.));
#35395=CARTESIAN_POINT('',(-0.332865020518126,-0.0586930840514225,0.));
#35396=CARTESIAN_POINT('',(-0.0722478752597442,0.101847162667754,0.));
#35397=CARTESIAN_POINT('',(-0.345475219623267,-0.0560969930232949,0.));
#35398=CARTESIAN_POINT('',(-0.0382251670489203,-0.119351276181666,0.));
#35399=CARTESIAN_POINT('',(-0.349967815369678,-0.0047463886666502,0.));
#35400=CARTESIAN_POINT('Origin',(0.,0.,0.));
#35401=CARTESIAN_POINT('',(-0.338,4.13930618111805E-17,0.));
#35402=CARTESIAN_POINT('',(-0.0407534494926875,0.117886816845732,0.));
#35403=CARTESIAN_POINT('',(-0.349967815369678,0.00474638866665025,0.));
#35404=CARTESIAN_POINT('',(-0.0664862087698295,-0.107681305378358,-2.77555756156289E-17));
#35405=CARTESIAN_POINT('',(-0.345475219623267,0.0560969930232949,0.));
#35406=CARTESIAN_POINT('Origin',(0.,0.,0.));
#35407=CARTESIAN_POINT('',(-0.332865020518126,0.0586930840514224,0.));
#35408=CARTESIAN_POINT('',(-0.0111111777379252,0.124933296243372,0.));
#35409=CARTESIAN_POINT('',(-0.343826816138341,0.0654455537387477,0.));
#35410=CARTESIAN_POINT('',(-0.0958175276338027,-0.087328249096412,2.77555756156289E-17));
#35411=CARTESIAN_POINT('',(-0.330485534147499,0.115235895966675,0.));
#35412=CARTESIAN_POINT('Origin',(0.,0.,0.));
#35413=CARTESIAN_POINT('',(-0.317616105825637,0.115602808444076,0.));
#35414=CARTESIAN_POINT('',(0.0142742316533668,0.125065132869389,-2.77555756156289E-17));
#35415=CARTESIAN_POINT('',(-0.327238813083405,0.124156188777542,0.));
#35416=CARTESIAN_POINT('',(-0.123130440725462,-0.0572705647603282,0.));
#35417=CARTESIAN_POINT('',(-0.305454212950408,0.170873414523285,0.));
#35418=CARTESIAN_POINT('Origin',(0.,0.,0.));
#35419=CARTESIAN_POINT('',(-0.29271658647914,0.169,0.));
#35420=CARTESIAN_POINT('',(0.0340022454231837,0.1209471067787,5.55111512312578E-17));
#35421=CARTESIAN_POINT('',(-0.300707824283758,0.179094400846393,0.));
#35422=CARTESIAN_POINT('',(-0.144969217443638,-0.017632059201444,0.));
#35423=CARTESIAN_POINT('',(-0.27114182006011,0.221319030845725,0.));
#35424=CARTESIAN_POINT('Origin',(0.,0.,0.));
#35425=CARTESIAN_POINT('',(-0.258923021774215,0.21726221207405,0.));
#35426=CARTESIAN_POINT('',(0.0477949519661669,0.115427383119028,-2.77555756156289E-17));
#35427=CARTESIAN_POINT('',(-0.265039980408751,0.228590920171666,0.));
#35428=CARTESIAN_POINT('',(-0.157932795372159,0.0302266501264093,0.));
#35429=CARTESIAN_POINT('',(-0.228590920171666,0.265039980408751,0.));
#35430=CARTESIAN_POINT('Origin',(0.,0.,0.));
#35431=CARTESIAN_POINT('',(-0.21726221207405,0.258923021774215,0.));
#35432=CARTESIAN_POINT('',(0.0564667261863714,0.111122533140651,0.));
#35433=CARTESIAN_POINT('',(-0.221319030845725,0.27114182006011,0.));
#35434=CARTESIAN_POINT('',(-0.15910830301132,0.0837683194406838,0.));
#35435=CARTESIAN_POINT('',(-0.179094400846393,0.300707824283758,0.));
#35436=CARTESIAN_POINT('Origin',(0.,0.,0.));
#35437=CARTESIAN_POINT('',(-0.169,0.29271658647914,0.));
#35438=CARTESIAN_POINT('',(0.0617507117308451,0.110042662678602,-2.77555756156289E-17));
#35439=CARTESIAN_POINT('',(-0.170873414523285,0.305454212950408,0.));
#35440=CARTESIAN_POINT('',(-0.146463392037742,0.139486807065864,2.77555756156289E-17));
#35441=CARTESIAN_POINT('',(-0.124156188777542,0.327238813083405,0.));
#35442=CARTESIAN_POINT('Origin',(0.,0.,0.));
#35443=CARTESIAN_POINT('',(-0.115602808444076,0.317616105825637,0.));
#35444=CARTESIAN_POINT('',(0.0660053371168799,0.113303664167723,0.));
#35445=CARTESIAN_POINT('',(-0.115235895966675,0.330485534147499,0.));
#35446=CARTESIAN_POINT('',(-0.119148812359806,0.193240277710374,-2.77555756156289E-17));
#35447=CARTESIAN_POINT('',(-0.0654455537387477,0.343826816138341,0.));
#35448=CARTESIAN_POINT('Origin',(0.,0.,0.));
#35449=CARTESIAN_POINT('',(-0.0586930840514224,0.332865020518126,0.));
#35450=CARTESIAN_POINT('',(0.0718388299416056,0.12096267524839,0.));
#35451=CARTESIAN_POINT('',(-0.0560969930232949,0.345475219623267,0.));
#35452=CARTESIAN_POINT('',(-0.0776729895490008,0.240672418360475,0.));
#35453=CARTESIAN_POINT('',(-0.00474638866665024,0.349967815369678,0.));
#35454=CARTESIAN_POINT('Origin',(0.,0.,0.));
#35455=CARTESIAN_POINT('',(2.06965309055903E-17,0.338,0.));
#35456=CARTESIAN_POINT('',(0.0816997840353174,0.13199750004727,0.));
#35457=CARTESIAN_POINT('',(0.00474638866665027,0.349967815369678,0.));
#35458=CARTESIAN_POINT('',(-0.0239253559329411,0.277673241580245,0.));
#35459=CARTESIAN_POINT('',(0.0560969930232949,0.345475219623267,0.));
#35460=CARTESIAN_POINT('Origin',(0.,0.,0.));
#35461=CARTESIAN_POINT('',(0.0586930840514225,0.332865020518126,0.));
#35462=CARTESIAN_POINT('',(0.0974860449318179,0.144432891105261,-2.77555756156289E-17));
#35463=CARTESIAN_POINT('',(0.0654455537387478,0.343826816138341,0.));
#35464=CARTESIAN_POINT('',(0.0389569509149426,0.300825860359951,5.55111512312578E-17));
#35465=CARTESIAN_POINT('',(0.115235895966675,0.330485534147499,0.));
#35466=CARTESIAN_POINT('Origin',(0.,0.,0.));
#35467=CARTESIAN_POINT('',(0.115602808444076,0.317616105825637,0.));
#35468=CARTESIAN_POINT('',(0.120221998005621,0.155598369638155,-2.77555756156289E-17));
#35469=CARTESIAN_POINT('',(0.124156188777542,0.327238813083405,0.));
#35470=CARTESIAN_POINT('',(0.106865818287004,0.307786834202281,2.77555756156289E-17));
#35471=CARTESIAN_POINT('',(0.170873414523285,0.305454212950408,0.));
#35472=CARTESIAN_POINT('Origin',(0.,0.,0.));
#35473=CARTESIAN_POINT('',(0.169,0.29271658647914,0.));
#35474=CARTESIAN_POINT('',(0.149846033266815,0.162485892386646,0.));
#35475=CARTESIAN_POINT('',(0.179094400846393,0.300707824283758,0.));
#35476=CARTESIAN_POINT('',(0.175112028053804,0.297555176742166,0.));
#35477=CARTESIAN_POINT('',(0.221319030845725,0.27114182006011,0.));
#35478=CARTESIAN_POINT('Origin',(0.,0.,0.));
#35479=CARTESIAN_POINT('',(0.21726221207405,0.258923021774215,0.));
#35480=CARTESIAN_POINT('',(0.185136525284291,0.162163144448502,0.));
#35481=CARTESIAN_POINT('',(0.228590920171666,0.265039980408751,0.));
#35482=CARTESIAN_POINT('',(0.238884451429285,0.27059799323454,2.77555756156289E-17));
#35483=CARTESIAN_POINT('',(0.265039980408751,0.228590920171666,0.));
#35484=CARTESIAN_POINT('Origin',(0.,0.,0.));
#35485=CARTESIAN_POINT('',(0.258923021774215,0.21726221207405,0.));
#35486=CARTESIAN_POINT('',(0.223787731003033,0.152191075116504,0.));
#35487=CARTESIAN_POINT('',(0.27114182006011,0.221319030845725,0.));
#35488=CARTESIAN_POINT('',(0.293726415855352,0.228817445176584,0.));
#35489=CARTESIAN_POINT('',(0.300707824283758,0.179094400846393,0.));
#35490=CARTESIAN_POINT('Origin',(0.,0.,0.));
#35491=CARTESIAN_POINT('',(0.29271658647914,0.169,0.));
#35492=CARTESIAN_POINT('',(0.262628621977131,0.130993375524403,0.));
#35493=CARTESIAN_POINT('',(0.305454212950408,0.170873414523285,0.));
#35494=CARTESIAN_POINT('',(0.335974944875694,0.175362318525856,0.));
#35495=CARTESIAN_POINT('',(0.327238813083405,0.124156188777542,0.));
#35496=CARTESIAN_POINT('Origin',(0.,0.,0.));
#35497=CARTESIAN_POINT('',(0.317616105825637,0.115602808444076,0.));
#35498=CARTESIAN_POINT('',(0.297960057644542,0.098131045930453,-2.77555756156289E-17));
#35499=CARTESIAN_POINT('',(0.330485534147499,0.115235895966675,0.));
#35500=CARTESIAN_POINT('',(0.363112879001896,0.114305677496039,-2.77555756156289E-17));
#35501=CARTESIAN_POINT('',(0.343826816138341,0.0654455537387478,0.));
#35502=CARTESIAN_POINT('Origin',(0.,0.,0.));
#35503=CARTESIAN_POINT('',(0.332865020518126,0.0586930840514224,0.));
#35504=CARTESIAN_POINT('',(0.325971007974539,0.0544463700697488,2.77555756156289E-17));
#35505=CARTESIAN_POINT('',(0.345475219623267,0.0560969930232949,0.));
#35506=CARTESIAN_POINT('',(0.37399413172781,0.050225738237446,0.));
#35507=CARTESIAN_POINT('',(0.349967815369678,0.00474638866665024,0.));
#35508=CARTESIAN_POINT('Origin',(0.,0.,0.));
#35509=CARTESIAN_POINT('',(0.338,0.,0.));
#35510=CARTESIAN_POINT('',(0.343184532857686,0.00205616541009999,0.));
#35511=CARTESIAN_POINT('',(0.349967815369678,-0.00474638866665023,0.));
#35512=CARTESIAN_POINT('',(0.368917292134828,-0.012261676877474,0.));
#35513=CARTESIAN_POINT('',(0.345475219623267,-0.0560969930232949,0.));
#35514=CARTESIAN_POINT('Origin',(0.,0.,0.));
#35515=CARTESIAN_POINT('',(0.332865020518126,-0.0586930840514225,0.));
#35516=CARTESIAN_POINT('',(0.346880142416816,-0.0558077582991534,0.));
#35517=CARTESIAN_POINT('',(0.343826816138341,-0.0654455537387478,0.));
#35518=CARTESIAN_POINT('',(0.349540660348596,-0.0689652836410913,2.77555756156289E-17));
#35519=CARTESIAN_POINT('Origin',(0.,0.,0.));
#35520=CARTESIAN_POINT('Origin',(0.,0.,0.201));
#35521=CARTESIAN_POINT('',(0.0866025403784438,-0.15,0.201));
#35522=CARTESIAN_POINT('',(-0.086602540378444,-0.15,0.201));
#35523=CARTESIAN_POINT('',(0.0433012701892219,-0.15,0.201));
#35524=CARTESIAN_POINT('Origin',(0.,0.,0.201));
#35525=CARTESIAN_POINT('Origin',(0.,0.,0.201));
#35526=CARTESIAN_POINT('',(-0.173205080756888,8.32667268468867E-17,0.201));
#35527=CARTESIAN_POINT('',(-0.108253175473055,-0.1125,0.201));
#35528=CARTESIAN_POINT('Origin',(0.,0.,0.201));
#35529=CARTESIAN_POINT('Origin',(0.,0.,0.201));
#35530=CARTESIAN_POINT('',(-0.0866025403784438,0.15,0.201));
#35531=CARTESIAN_POINT('',(-0.151554445662277,0.0375,0.201));
#35532=CARTESIAN_POINT('Origin',(0.,0.,0.201));
#35533=CARTESIAN_POINT('Origin',(0.,0.,0.201));
#35534=CARTESIAN_POINT('',(0.0866025403784439,0.15,0.201));
#35535=CARTESIAN_POINT('',(-0.0433012701892219,0.15,0.201));
#35536=CARTESIAN_POINT('Origin',(0.,0.,0.201));
#35537=CARTESIAN_POINT('Origin',(0.,0.,0.201));
#35538=CARTESIAN_POINT('',(0.173205080756888,0.,0.201));
#35539=CARTESIAN_POINT('',(0.108253175473055,0.1125,0.201));
#35540=CARTESIAN_POINT('Origin',(0.,0.,0.201));
#35541=CARTESIAN_POINT('Origin',(0.,0.,0.201));
#35542=CARTESIAN_POINT('',(0.151554445662277,-0.0375,0.201));
#35543=CARTESIAN_POINT('Origin',(0.,0.,0.201));
#35544=CARTESIAN_POINT('Origin',(0.,0.,0.148538475772934));
#35545=CARTESIAN_POINT('',(0.,0.,0.0960769515458673));
#35546=CARTESIAN_POINT('',(-0.171554298747513,-2.1009342284111E-17,0.2));
#35547=CARTESIAN_POINT('',(-0.0866025403784439,-1.06057523872491E-17,0.148538475772934));
#35548=CARTESIAN_POINT('',(-0.171529756258877,-0.0029017471497188,0.2));
#35549=CARTESIAN_POINT('Origin',(0.,0.,0.2));
#35550=CARTESIAN_POINT('Ctrl Pts',(-0.173205080756888,-1.52655665885959E-16,
0.201));
#35551=CARTESIAN_POINT('Ctrl Pts',(-0.172363407600995,-0.00145782066937349,
0.200490136704233));
#35552=CARTESIAN_POINT('Ctrl Pts',(-0.171529756258877,-0.00290174714971882,
0.2));
#35553=CARTESIAN_POINT('',(-0.0882778648764544,-0.147098252850281,0.2));
#35554=CARTESIAN_POINT('Ctrl Pts',(-0.0882778648764544,-0.147098252850281,
0.2));
#35555=CARTESIAN_POINT('Ctrl Pts',(-0.0874442135343418,-0.148542179330618,
0.20049013670423));
#35556=CARTESIAN_POINT('Ctrl Pts',(-0.0866025403784441,-0.15,0.201));
#35557=CARTESIAN_POINT('',(-0.0832518913824231,-0.15,0.2));
#35558=CARTESIAN_POINT('Origin',(0.,0.,0.2));
#35559=CARTESIAN_POINT('Ctrl Pts',(-0.0866025403784439,-0.15,0.201));
#35560=CARTESIAN_POINT('Ctrl Pts',(-0.0849191940666532,-0.15,0.200490136704232));
#35561=CARTESIAN_POINT('Ctrl Pts',(-0.0832518913824231,-0.15,0.2));
#35562=CARTESIAN_POINT('',(0.0832518913824231,-0.15,0.2));
#35563=CARTESIAN_POINT('Ctrl Pts',(0.0832518913824231,-0.15,0.2));
#35564=CARTESIAN_POINT('Ctrl Pts',(0.084919194066652,-0.15,0.200490136704231));
#35565=CARTESIAN_POINT('Ctrl Pts',(0.0866025403784438,-0.15,0.201));
#35566=CARTESIAN_POINT('',(0.0882778648764543,-0.147098252850281,0.2));
#35567=CARTESIAN_POINT('Origin',(0.,0.,0.2));
#35568=CARTESIAN_POINT('Ctrl Pts',(0.0866025403784439,-0.15,0.201));
#35569=CARTESIAN_POINT('Ctrl Pts',(0.0874442135343394,-0.148542179330622,
0.200490136704231));
#35570=CARTESIAN_POINT('Ctrl Pts',(0.0882778648764543,-0.147098252850281,
0.2));
#35571=CARTESIAN_POINT('',(0.171529756258877,-0.00290174714971884,0.2));
#35572=CARTESIAN_POINT('Ctrl Pts',(0.171529756258877,-0.00290174714971883,
0.2));
#35573=CARTESIAN_POINT('Ctrl Pts',(0.172363407600991,-0.00145782066937972,
0.200490136704231));
#35574=CARTESIAN_POINT('Ctrl Pts',(0.173205080756888,-1.38777878078145E-17,
0.201));
#35575=CARTESIAN_POINT('',(0.171529756258877,0.00290174714971882,0.2));
#35576=CARTESIAN_POINT('Origin',(0.,0.,0.2));
#35577=CARTESIAN_POINT('Ctrl Pts',(0.173205080756888,-4.16333634234434E-17,
0.201));
#35578=CARTESIAN_POINT('Ctrl Pts',(0.172363407600995,0.00145782066937251,
0.200490136704233));
#35579=CARTESIAN_POINT('Ctrl Pts',(0.171529756258877,0.00290174714971887,
0.2));
#35580=CARTESIAN_POINT('',(0.0882778648764543,0.147098252850281,0.2));
#35581=CARTESIAN_POINT('Ctrl Pts',(0.0882778648764543,0.147098252850281,
0.2));
#35582=CARTESIAN_POINT('Ctrl Pts',(0.0874442135343416,0.148542179330618,
0.20049013670423));
#35583=CARTESIAN_POINT('Ctrl Pts',(0.0866025403784439,0.15,0.201));
#35584=CARTESIAN_POINT('',(0.0832518913824231,0.15,0.2));
#35585=CARTESIAN_POINT('Origin',(0.,0.,0.2));
#35586=CARTESIAN_POINT('Ctrl Pts',(0.0866025403784438,0.15,0.201));
#35587=CARTESIAN_POINT('Ctrl Pts',(0.0849191940666536,0.15,0.200490136704232));
#35588=CARTESIAN_POINT('Ctrl Pts',(0.0832518913824231,0.15,0.2));
#35589=CARTESIAN_POINT('',(-0.0832518913824231,0.15,0.2));
#35590=CARTESIAN_POINT('Ctrl Pts',(-0.0832518913824231,0.15,0.2));
#35591=CARTESIAN_POINT('Ctrl Pts',(-0.0849191940666509,0.15,0.200490136704231));
#35592=CARTESIAN_POINT('Ctrl Pts',(-0.0866025403784438,0.15,0.201));
#35593=CARTESIAN_POINT('',(-0.0882778648764542,0.147098252850281,0.2));
#35594=CARTESIAN_POINT('Origin',(0.,0.,0.2));
#35595=CARTESIAN_POINT('Ctrl Pts',(-0.0866025403784439,0.15,0.201));
#35596=CARTESIAN_POINT('Ctrl Pts',(-0.0874442135343377,0.148542179330625,
0.200490136704232));
#35597=CARTESIAN_POINT('Ctrl Pts',(-0.0882778648764542,0.147098252850281,
0.2));
#35598=CARTESIAN_POINT('',(-0.171529756258877,0.00290174714971888,0.2));
#35599=CARTESIAN_POINT('Ctrl Pts',(-0.171529756258877,0.00290174714971886,
0.2));
#35600=CARTESIAN_POINT('Ctrl Pts',(-0.172363407600993,0.00145782066937643,
0.200490136704232));
#35601=CARTESIAN_POINT('Ctrl Pts',(-0.173205080756888,1.52655665885959E-16,
0.201));
#35602=CARTESIAN_POINT('Origin',(0.,0.,0.2));
#35603=CARTESIAN_POINT('Origin',(-0.173205080756888,2.77555756156289E-17,
0.4));
#35604=CARTESIAN_POINT('',(-0.0866025403784438,0.15,0.4));
#35605=CARTESIAN_POINT('',(-0.0866025403784438,0.15,0.4));
#35606=CARTESIAN_POINT('',(-0.173205080756888,2.12115047744981E-17,0.4));
#35607=CARTESIAN_POINT('',(-0.151554445662277,0.0375,0.4));
#35608=CARTESIAN_POINT('',(-0.173205080756888,2.12115047744981E-17,0.4));
#35609=CARTESIAN_POINT('Origin',(-0.173205080756888,2.77555756156289E-17,
0.4));
#35610=CARTESIAN_POINT('',(-0.173205080756888,2.77555756156289E-17,0.2));
#35611=CARTESIAN_POINT('',(-0.173205080756888,2.12115047744981E-17,0.4));
#35612=CARTESIAN_POINT('',(-0.0866025403784438,0.15,0.2));
#35613=CARTESIAN_POINT('Origin',(-0.0866025403784438,0.15,0.4));
#35614=CARTESIAN_POINT('',(0.0866025403784439,0.15,0.4));
#35615=CARTESIAN_POINT('',(0.0866025403784439,0.15,0.4));
#35616=CARTESIAN_POINT('',(-0.0433012701892219,0.15,0.4));
#35617=CARTESIAN_POINT('Origin',(-0.0866025403784438,0.15,0.4));
#35618=CARTESIAN_POINT('',(0.0866025403784439,0.15,0.2));
#35619=CARTESIAN_POINT('',(0.0866025403784439,0.15,0.2));
#35620=CARTESIAN_POINT('',(0.0866025403784439,0.15,0.4));
#35621=CARTESIAN_POINT('Origin',(-0.0866025403784438,0.15,0.4));
#35622=CARTESIAN_POINT('',(-0.0866025403784438,0.15,0.2));
#35623=CARTESIAN_POINT('',(-0.0866025403784438,0.15,0.4));
#35624=CARTESIAN_POINT('',(0.0866025403784439,0.15,0.2));
#35625=CARTESIAN_POINT('Origin',(-0.0866025403784439,-0.15,0.4));
#35626=CARTESIAN_POINT('',(-0.0866025403784439,-0.15,0.4));
#35627=CARTESIAN_POINT('',(-0.108253175473055,-0.1125,0.4));
#35628=CARTESIAN_POINT('',(-0.0866025403784439,-0.15,0.4));
#35629=CARTESIAN_POINT('Origin',(-0.0866025403784439,-0.15,0.4));
#35630=CARTESIAN_POINT('',(-0.0866025403784439,-0.15,0.2));
#35631=CARTESIAN_POINT('',(-0.0866025403784439,-0.15,0.4));
#35632=CARTESIAN_POINT('',(-0.173205080756888,2.12115047744981E-17,0.2));
#35633=CARTESIAN_POINT('Origin',(0.0866025403784439,0.15,0.4));
#35634=CARTESIAN_POINT('',(0.173205080756888,0.,0.4));
#35635=CARTESIAN_POINT('',(0.173205080756888,0.,0.4));
#35636=CARTESIAN_POINT('',(0.108253175473055,0.1125,0.4));
#35637=CARTESIAN_POINT('Origin',(0.0866025403784439,0.15,0.4));
#35638=CARTESIAN_POINT('',(0.173205080756888,0.,0.2));
#35639=CARTESIAN_POINT('',(0.173205080756888,0.,0.2));
#35640=CARTESIAN_POINT('',(0.173205080756888,0.,0.4));
#35641=CARTESIAN_POINT('Origin',(0.0866025403784439,0.15,0.4));
#35642=CARTESIAN_POINT('',(0.173205080756888,0.,0.2));
#35643=CARTESIAN_POINT('Origin',(0.,2.77555756156289E-17,0.2));
#35644=CARTESIAN_POINT('',(-0.0866025403784438,0.15,0.2));
#35645=CARTESIAN_POINT('Origin',(0.,2.77555756156289E-17,0.2));
#35646=CARTESIAN_POINT('Origin',(0.,2.77555756156289E-17,0.2));
#35647=CARTESIAN_POINT('',(0.0866025403784439,-0.15,0.2));
#35648=CARTESIAN_POINT('Origin',(0.,2.77555756156289E-17,0.2));
#35649=CARTESIAN_POINT('',(0.0866025403784439,-0.15,0.2));
#35650=CARTESIAN_POINT('',(-0.0866025403784439,-0.15,0.2));
#35651=CARTESIAN_POINT('',(0.0866025403784439,-0.15,0.2));
#35652=CARTESIAN_POINT('Origin',(0.,2.77555756156289E-17,0.2));
#35653=CARTESIAN_POINT('',(-0.0866025403784439,-0.15,0.2));
#35654=CARTESIAN_POINT('Origin',(0.,2.77555756156289E-17,0.2));
#35655=CARTESIAN_POINT('',(-0.173205080756888,2.12115047744981E-17,0.2));
#35656=CARTESIAN_POINT('Origin',(0.173205080756888,0.,0.4));
#35657=CARTESIAN_POINT('',(0.0866025403784439,-0.15,0.4));
#35658=CARTESIAN_POINT('',(0.0866025403784439,-0.15,0.4));
#35659=CARTESIAN_POINT('',(0.151554445662277,-0.0375,0.4));
#35660=CARTESIAN_POINT('Origin',(0.173205080756888,0.,0.4));
#35661=CARTESIAN_POINT('',(0.0866025403784439,-0.15,0.4));
#35662=CARTESIAN_POINT('Origin',(0.173205080756888,0.,0.4));
#35663=CARTESIAN_POINT('Origin',(0.0866025403784439,-0.15,0.4));
#35664=CARTESIAN_POINT('Origin',(0.0866025403784439,-0.15,0.4));
#35665=CARTESIAN_POINT('',(0.0433012701892219,-0.15,0.4));
#35666=CARTESIAN_POINT('Origin',(-0.173205080756888,2.77555756156289E-17,
0.4));
#35667=CARTESIAN_POINT('Origin',(-0.0866025403784439,-0.15,0.4));
#35668=CARTESIAN_POINT('Origin',(0.0866025403784439,-0.15,0.4));
#35669=CARTESIAN_POINT('Origin',(0.317616105825637,-0.115602808444076,0.4));
#35670=CARTESIAN_POINT('',(0.317616105825637,-0.115602808444076,0.372));
#35671=CARTESIAN_POINT('',(0.330485534147499,-0.115235895966675,0.36));
#35672=CARTESIAN_POINT('Ctrl Pts',(0.317616105825637,-0.115602808444076,
0.372));
#35673=CARTESIAN_POINT('Ctrl Pts',(0.32393858660004,-0.115422552023493,
0.366120462798036));
#35674=CARTESIAN_POINT('Ctrl Pts',(0.330485534147499,-0.115235895966675,
0.36));
#35675=CARTESIAN_POINT('',(0.317616105825637,-0.115602808444076,0.4));
#35676=CARTESIAN_POINT('',(0.330485534147499,-0.115235895966675,0.18));
#35677=CARTESIAN_POINT('Origin',(0.358996892846452,-0.152385140110817,0.4));
#35678=CARTESIAN_POINT('',(0.327238813083405,-0.124156188777542,0.36));
#35679=CARTESIAN_POINT('Ctrl Pts',(0.327238813083405,-0.124156188777541,
0.36));
#35680=CARTESIAN_POINT('Ctrl Pts',(0.322343540495881,-0.119804905177671,
0.366120462798032));
#35681=CARTESIAN_POINT('Ctrl Pts',(0.317616105825637,-0.115602808444076,
0.372));
#35682=CARTESIAN_POINT('',(0.327238813083405,-0.124156188777542,0.18));
#35683=CARTESIAN_POINT('Origin',(0.258923021774215,-0.21726221207405,0.4));
#35684=CARTESIAN_POINT('',(0.258923021774215,-0.21726221207405,0.372));
#35685=CARTESIAN_POINT('',(0.27114182006011,-0.221319030845725,0.36));
#35686=CARTESIAN_POINT('Ctrl Pts',(0.258923021774215,-0.21726221207405,
0.372));
#35687=CARTESIAN_POINT('Ctrl Pts',(0.264925861629792,-0.219255242226416,
0.36612046279803));
#35688=CARTESIAN_POINT('Ctrl Pts',(0.27114182006011,-0.221319030845725,
0.36));
#35689=CARTESIAN_POINT('',(0.258923021774215,-0.21726221207405,0.4));
#35690=CARTESIAN_POINT('',(0.27114182006011,-0.221319030845725,0.18));
#35691=CARTESIAN_POINT('Origin',(0.285227943631477,-0.265979360424374,0.4));
#35692=CARTESIAN_POINT('',(0.265039980408751,-0.228590920171666,0.36));
#35693=CARTESIAN_POINT('Ctrl Pts',(0.265039980408751,-0.228590920171666,
0.36));
#35694=CARTESIAN_POINT('Ctrl Pts',(0.261928155521996,-0.222827769249915,
0.366120462798034));
#35695=CARTESIAN_POINT('Ctrl Pts',(0.258923021774215,-0.21726221207405,
0.372));
#35696=CARTESIAN_POINT('',(0.265039980408751,-0.228590920171666,0.18));
#35697=CARTESIAN_POINT('Origin',(0.169,-0.29271658647914,0.4));
#35698=CARTESIAN_POINT('',(0.169,-0.29271658647914,0.372));
#35699=CARTESIAN_POINT('',(0.179094400846393,-0.300707824283758,0.36));
#35700=CARTESIAN_POINT('Ctrl Pts',(0.169,-0.29271658647914,0.372));
#35701=CARTESIAN_POINT('Ctrl Pts',(0.173959167857677,-0.296642514354085,
0.366120462798034));
#35702=CARTESIAN_POINT('Ctrl Pts',(0.179094400846393,-0.300707824283758,
0.36));
#35703=CARTESIAN_POINT('',(0.169,-0.29271658647914,0.4));
#35704=CARTESIAN_POINT('',(0.179094400846393,-0.300707824283758,0.18));
#35705=CARTESIAN_POINT('Origin',(0.177056294898423,-0.347492544433464,0.4));
#35706=CARTESIAN_POINT('',(0.170873414523285,-0.305454212950408,0.36));
#35707=CARTESIAN_POINT('Ctrl Pts',(0.170873414523285,-0.305454212950408,
0.36));
#35708=CARTESIAN_POINT('Ctrl Pts',(0.169920369344289,-0.298974315762995,
0.366120462798031));
#35709=CARTESIAN_POINT('Ctrl Pts',(0.169,-0.29271658647914,0.372));
#35710=CARTESIAN_POINT('',(0.170873414523285,-0.305454212950408,0.18));
#35711=CARTESIAN_POINT('Origin',(0.0586930840514223,-0.332865020518126,
0.4));
#35712=CARTESIAN_POINT('',(0.0586930840514223,-0.332865020518126,0.372));
#35713=CARTESIAN_POINT('',(0.0654455537387477,-0.343826816138341,0.36));
#35714=CARTESIAN_POINT('Ctrl Pts',(0.0586930840514223,-0.332865020518126,
0.372));
#35715=CARTESIAN_POINT('Ctrl Pts',(0.062010431078043,-0.338250321273404,
0.366120462798039));
#35716=CARTESIAN_POINT('Ctrl Pts',(0.0654455537387476,-0.343826816138341,
0.36));
#35717=CARTESIAN_POINT('',(0.0586930840514223,-0.332865020518126,0.4));
#35718=CARTESIAN_POINT('',(0.0654455537387477,-0.343826816138341,0.18));
#35719=CARTESIAN_POINT('Origin',(0.0475290439280076,-0.387092999140116,
0.4));
#35720=CARTESIAN_POINT('',(0.0560969930232948,-0.345475219623267,0.36));
#35721=CARTESIAN_POINT('Ctrl Pts',(0.0560969930232948,-0.345475219623267,
0.36));
#35722=CARTESIAN_POINT('Ctrl Pts',(0.0574176788660909,-0.339060147404089,
0.36612046279803));
#35723=CARTESIAN_POINT('Ctrl Pts',(0.0586930840514223,-0.332865020518126,
0.372));
#35724=CARTESIAN_POINT('',(0.0560969930232948,-0.345475219623267,0.18));
#35725=CARTESIAN_POINT('Origin',(-0.0586930840514224,-0.332865020518126,
0.4));
#35726=CARTESIAN_POINT('',(-0.0586930840514225,-0.332865020518126,0.372));
#35727=CARTESIAN_POINT('',(-0.0560969930232949,-0.345475219623267,0.36));
#35728=CARTESIAN_POINT('Ctrl Pts',(-0.0586930840514225,-0.332865020518126,
0.372));
#35729=CARTESIAN_POINT('Ctrl Pts',(-0.0574176788660934,-0.339060147404077,
0.366120462798041));
#35730=CARTESIAN_POINT('Ctrl Pts',(-0.0560969930232949,-0.345475219623267,
0.36));
#35731=CARTESIAN_POINT('',(-0.0586930840514224,-0.332865020518126,0.4));
#35732=CARTESIAN_POINT('',(-0.0560969930232949,-0.345475219623267,0.18));
#35733=CARTESIAN_POINT('Origin',(-0.0877309111941074,-0.380004325266242,
0.4));
#35734=CARTESIAN_POINT('',(-0.0654455537387478,-0.343826816138341,0.36));
#35735=CARTESIAN_POINT('Ctrl Pts',(-0.0654455537387477,-0.343826816138341,
0.36));
#35736=CARTESIAN_POINT('Ctrl Pts',(-0.062010431078045,-0.338250321273407,
0.366120462798035));
#35737=CARTESIAN_POINT('Ctrl Pts',(-0.0586930840514225,-0.332865020518126,
0.372));
#35738=CARTESIAN_POINT('',(-0.0654455537387478,-0.343826816138341,0.18));
#35739=CARTESIAN_POINT('Origin',(-0.169,-0.29271658647914,0.4));
#35740=CARTESIAN_POINT('',(-0.169,-0.29271658647914,0.372));
#35741=CARTESIAN_POINT('',(-0.170873414523286,-0.305454212950408,0.36));
#35742=CARTESIAN_POINT('Ctrl Pts',(-0.169,-0.29271658647914,0.372));
#35743=CARTESIAN_POINT('Ctrl Pts',(-0.16992036934429,-0.298974315762997,
0.36612046279803));
#35744=CARTESIAN_POINT('Ctrl Pts',(-0.170873414523285,-0.305454212950408,
0.36));
#35745=CARTESIAN_POINT('',(-0.169,-0.29271658647914,0.4));
#35746=CARTESIAN_POINT('',(-0.170873414523286,-0.305454212950408,0.18));
#35747=CARTESIAN_POINT('Origin',(-0.212409223655861,-0.327081521498715,
0.4));
#35748=CARTESIAN_POINT('',(-0.179094400846393,-0.300707824283758,0.36));
#35749=CARTESIAN_POINT('Ctrl Pts',(-0.179094400846393,-0.300707824283758,
0.36));
#35750=CARTESIAN_POINT('Ctrl Pts',(-0.173959167857676,-0.296642514354083,
0.366120462798036));
#35751=CARTESIAN_POINT('Ctrl Pts',(-0.169,-0.29271658647914,0.372));
#35752=CARTESIAN_POINT('',(-0.179094400846393,-0.300707824283758,0.18));
#35753=CARTESIAN_POINT('Origin',(-0.258923021774215,-0.21726221207405,0.4));
#35754=CARTESIAN_POINT('',(-0.258923021774215,-0.21726221207405,0.372));
#35755=CARTESIAN_POINT('',(-0.265039980408751,-0.228590920171666,0.36));
#35756=CARTESIAN_POINT('Ctrl Pts',(-0.258923021774215,-0.21726221207405,
0.372));
#35757=CARTESIAN_POINT('Ctrl Pts',(-0.261928155521997,-0.222827769249916,
0.366120462798033));
#35758=CARTESIAN_POINT('Ctrl Pts',(-0.265039980408751,-0.228590920171666,
0.36));
#35759=CARTESIAN_POINT('',(-0.258923021774215,-0.21726221207405,0.4));
#35760=CARTESIAN_POINT('',(-0.265039980408751,-0.228590920171666,0.18));
#35761=CARTESIAN_POINT('Origin',(-0.311467848918444,-0.234707859029299,
0.4));
#35762=CARTESIAN_POINT('',(-0.27114182006011,-0.221319030845725,0.36));
#35763=CARTESIAN_POINT('Ctrl Pts',(-0.27114182006011,-0.221319030845725,
0.36));
#35764=CARTESIAN_POINT('Ctrl Pts',(-0.264925861629788,-0.219255242226415,
0.366120462798033));
#35765=CARTESIAN_POINT('Ctrl Pts',(-0.258923021774215,-0.21726221207405,
0.372));
#35766=CARTESIAN_POINT('',(-0.27114182006011,-0.221319030845725,0.18));
#35767=CARTESIAN_POINT('Origin',(-0.317616105825637,-0.115602808444076,
0.4));
#35768=CARTESIAN_POINT('',(-0.317616105825637,-0.115602808444076,0.372));
#35769=CARTESIAN_POINT('',(-0.327238813083405,-0.124156188777542,0.36));
#35770=CARTESIAN_POINT('Ctrl Pts',(-0.317616105825637,-0.115602808444076,
0.372));
#35771=CARTESIAN_POINT('Ctrl Pts',(-0.322343540495879,-0.119804905177669,
0.366120462798034));
#35772=CARTESIAN_POINT('Ctrl Pts',(-0.327238813083405,-0.124156188777541,
0.36));
#35773=CARTESIAN_POINT('',(-0.317616105825637,-0.115602808444076,0.4));
#35774=CARTESIAN_POINT('',(-0.327238813083405,-0.124156188777542,0.18));
#35775=CARTESIAN_POINT('Origin',(-0.372958854825584,-0.114024964841867,
0.4));
#35776=CARTESIAN_POINT('',(-0.330485534147499,-0.115235895966675,0.36));
#35777=CARTESIAN_POINT('Ctrl Pts',(-0.330485534147499,-0.115235895966675,
0.36));
#35778=CARTESIAN_POINT('Ctrl Pts',(-0.32393858660004,-0.115422552023493,
0.366120462798036));
#35779=CARTESIAN_POINT('Ctrl Pts',(-0.317616105825637,-0.115602808444076,
0.372));
#35780=CARTESIAN_POINT('',(-0.330485534147499,-0.115235895966675,0.18));
#35781=CARTESIAN_POINT('Origin',(-0.338,4.13930618111805E-17,0.4));
#35782=CARTESIAN_POINT('',(-0.338,4.13930618111805E-17,0.372));
#35783=CARTESIAN_POINT('',(-0.349967815369678,-0.0047463886666502,0.36));
#35784=CARTESIAN_POINT('Ctrl Pts',(-0.338,4.13930618111805E-17,0.372));
#35785=CARTESIAN_POINT('Ctrl Pts',(-0.343879537201965,-0.00233180140890689,
0.366120462798035));
#35786=CARTESIAN_POINT('Ctrl Pts',(-0.349967815369678,-0.00474638866665013,
0.36));
#35787=CARTESIAN_POINT('',(-0.338,4.13930618111805E-17,0.4));
#35788=CARTESIAN_POINT('',(-0.349967815369678,-0.0047463886666502,0.18));
#35789=CARTESIAN_POINT('Origin',(-0.389465518554284,0.0204110229347481,
0.4));
#35790=CARTESIAN_POINT('',(-0.349967815369678,0.00474638866665025,0.36));
#35791=CARTESIAN_POINT('Ctrl Pts',(-0.349967815369678,0.00474638866665024,
0.36));
#35792=CARTESIAN_POINT('Ctrl Pts',(-0.343879537201956,0.00233180140890372,
0.366120462798043));
#35793=CARTESIAN_POINT('Ctrl Pts',(-0.338,4.13930618111805E-17,0.372));
#35794=CARTESIAN_POINT('',(-0.349967815369678,0.00474638866665025,0.18));
#35795=CARTESIAN_POINT('Origin',(-0.332865020518126,0.0586930840514224,
0.4));
#35796=CARTESIAN_POINT('',(-0.332865020518126,0.0586930840514224,0.372));
#35797=CARTESIAN_POINT('',(-0.345475219623267,0.0560969930232949,0.36));
#35798=CARTESIAN_POINT('Ctrl Pts',(-0.332865020518126,0.0586930840514224,
0.372));
#35799=CARTESIAN_POINT('Ctrl Pts',(-0.33906014740408,0.0574176788660928,
0.366120462798038));
#35800=CARTESIAN_POINT('Ctrl Pts',(-0.345475219623267,0.0560969930232949,
0.36));
#35801=CARTESIAN_POINT('',(-0.332865020518126,0.0586930840514224,0.4));
#35802=CARTESIAN_POINT('',(-0.345475219623267,0.0560969930232949,0.18));
#35803=CARTESIAN_POINT('Origin',(-0.380004325266242,0.0877309111941074,
0.4));
#35804=CARTESIAN_POINT('',(-0.343826816138341,0.0654455537387477,0.36));
#35805=CARTESIAN_POINT('Ctrl Pts',(-0.343826816138341,0.0654455537387478,
0.36));
#35806=CARTESIAN_POINT('Ctrl Pts',(-0.338250321273404,0.0620104310780433,
0.366120462798038));
#35807=CARTESIAN_POINT('Ctrl Pts',(-0.332865020518126,0.0586930840514224,
0.372));
#35808=CARTESIAN_POINT('',(-0.343826816138341,0.0654455537387477,0.18));
#35809=CARTESIAN_POINT('Origin',(-0.29271658647914,0.169,0.4));
#35810=CARTESIAN_POINT('',(-0.29271658647914,0.169,0.372));
#35811=CARTESIAN_POINT('',(-0.305454212950408,0.170873414523285,0.36));
#35812=CARTESIAN_POINT('Ctrl Pts',(-0.29271658647914,0.169,0.372));
#35813=CARTESIAN_POINT('Ctrl Pts',(-0.298974315762988,0.169920369344288,
0.366120462798038));
#35814=CARTESIAN_POINT('Ctrl Pts',(-0.305454212950408,0.170873414523285,
0.36));
#35815=CARTESIAN_POINT('',(-0.29271658647914,0.169,0.4));
#35816=CARTESIAN_POINT('',(-0.305454212950408,0.170873414523285,0.18));
#35817=CARTESIAN_POINT('Origin',(-0.327081521498715,0.212409223655861,0.4));
#35818=CARTESIAN_POINT('',(-0.300707824283758,0.179094400846393,0.36));
#35819=CARTESIAN_POINT('Ctrl Pts',(-0.300707824283758,0.179094400846393,
0.36));
#35820=CARTESIAN_POINT('Ctrl Pts',(-0.296642514354079,0.17395916785767,
0.366120462798042));
#35821=CARTESIAN_POINT('Ctrl Pts',(-0.29271658647914,0.169,0.372));
#35822=CARTESIAN_POINT('',(-0.300707824283758,0.179094400846393,0.18));
#35823=CARTESIAN_POINT('Origin',(-0.21726221207405,0.258923021774215,0.4));
#35824=CARTESIAN_POINT('',(-0.21726221207405,0.258923021774215,0.372));
#35825=CARTESIAN_POINT('',(-0.228590920171666,0.265039980408751,0.36));
#35826=CARTESIAN_POINT('Ctrl Pts',(-0.21726221207405,0.258923021774215,
0.372));
#35827=CARTESIAN_POINT('Ctrl Pts',(-0.222827769249908,0.261928155521993,
0.366120462798042));
#35828=CARTESIAN_POINT('Ctrl Pts',(-0.228590920171666,0.265039980408751,
0.36));
#35829=CARTESIAN_POINT('',(-0.21726221207405,0.258923021774215,0.4));
#35830=CARTESIAN_POINT('',(-0.228590920171666,0.265039980408751,0.18));
#35831=CARTESIAN_POINT('Origin',(-0.234707859029299,0.311467848918444,0.4));
#35832=CARTESIAN_POINT('',(-0.221319030845725,0.27114182006011,0.36));
#35833=CARTESIAN_POINT('Ctrl Pts',(-0.221319030845725,0.27114182006011,
0.36));
#35834=CARTESIAN_POINT('Ctrl Pts',(-0.219255242226413,0.264925861629782,
0.366120462798039));
#35835=CARTESIAN_POINT('Ctrl Pts',(-0.21726221207405,0.258923021774215,
0.372));
#35836=CARTESIAN_POINT('',(-0.221319030845725,0.27114182006011,0.18));
#35837=CARTESIAN_POINT('Origin',(-0.115602808444076,0.317616105825637,0.4));
#35838=CARTESIAN_POINT('',(-0.115602808444076,0.317616105825637,0.372));
#35839=CARTESIAN_POINT('',(-0.124156188777542,0.327238813083405,0.36));
#35840=CARTESIAN_POINT('Ctrl Pts',(-0.115602808444076,0.317616105825637,
0.372));
#35841=CARTESIAN_POINT('Ctrl Pts',(-0.119804905177669,0.322343540495879,
0.366120462798034));
#35842=CARTESIAN_POINT('Ctrl Pts',(-0.124156188777542,0.327238813083405,
0.36));
#35843=CARTESIAN_POINT('',(-0.115602808444076,0.317616105825637,0.4));
#35844=CARTESIAN_POINT('',(-0.124156188777542,0.327238813083405,0.18));
#35845=CARTESIAN_POINT('Origin',(-0.114024964841867,0.372958854825584,0.4));
#35846=CARTESIAN_POINT('',(-0.115235895966675,0.330485534147499,0.36));
#35847=CARTESIAN_POINT('Ctrl Pts',(-0.115235895966675,0.330485534147499,
0.36));
#35848=CARTESIAN_POINT('Ctrl Pts',(-0.115422552023493,0.323938586600039,
0.366120462798037));
#35849=CARTESIAN_POINT('Ctrl Pts',(-0.115602808444076,0.317616105825637,
0.372));
#35850=CARTESIAN_POINT('',(-0.115235895966675,0.330485534147499,0.18));
#35851=CARTESIAN_POINT('Origin',(2.06965309055903E-17,0.338,0.4));
#35852=CARTESIAN_POINT('',(2.06965309055903E-17,0.338,0.372));
#35853=CARTESIAN_POINT('',(-0.00474638866665024,0.349967815369678,0.36));
#35854=CARTESIAN_POINT('Ctrl Pts',(2.06965309055903E-17,0.338,0.372));
#35855=CARTESIAN_POINT('Ctrl Pts',(-0.00233180140890855,0.343879537201969,
0.366120462798031));
#35856=CARTESIAN_POINT('Ctrl Pts',(-0.00474638866665021,0.349967815369678,
0.36));
#35857=CARTESIAN_POINT('',(2.06965309055903E-17,0.338,0.4));
#35858=CARTESIAN_POINT('',(-0.00474638866665024,0.349967815369678,0.18));
#35859=CARTESIAN_POINT('Origin',(0.0204110229347481,0.389465518554284,0.4));
#35860=CARTESIAN_POINT('',(0.00474638866665027,0.349967815369678,0.36));
#35861=CARTESIAN_POINT('Ctrl Pts',(0.00474638866665025,0.349967815369678,
0.36));
#35862=CARTESIAN_POINT('Ctrl Pts',(0.00233180140890579,0.343879537201962,
0.366120462798038));
#35863=CARTESIAN_POINT('Ctrl Pts',(2.06965309055903E-17,0.338,0.372));
#35864=CARTESIAN_POINT('',(0.00474638866665027,0.349967815369678,0.18));
#35865=CARTESIAN_POINT('Origin',(0.115602808444076,0.317616105825637,0.4));
#35866=CARTESIAN_POINT('',(0.115602808444076,0.317616105825637,0.372));
#35867=CARTESIAN_POINT('',(0.115235895966675,0.330485534147499,0.36));
#35868=CARTESIAN_POINT('Ctrl Pts',(0.115602808444076,0.317616105825637,
0.372));
#35869=CARTESIAN_POINT('Ctrl Pts',(0.115422552023493,0.323938586600037,
0.366120462798039));
#35870=CARTESIAN_POINT('Ctrl Pts',(0.115235895966675,0.330485534147499,
0.36));
#35871=CARTESIAN_POINT('',(0.115602808444076,0.317616105825637,0.4));
#35872=CARTESIAN_POINT('',(0.115235895966675,0.330485534147499,0.18));
#35873=CARTESIAN_POINT('Origin',(0.152385140110817,0.358996892846452,0.4));
#35874=CARTESIAN_POINT('',(0.124156188777542,0.327238813083405,0.36));
#35875=CARTESIAN_POINT('Ctrl Pts',(0.124156188777542,0.327238813083405,
0.36));
#35876=CARTESIAN_POINT('Ctrl Pts',(0.119804905177668,0.322343540495878,
0.366120462798036));
#35877=CARTESIAN_POINT('Ctrl Pts',(0.115602808444076,0.317616105825637,
0.372));
#35878=CARTESIAN_POINT('',(0.124156188777542,0.327238813083405,0.18));
#35879=CARTESIAN_POINT('Origin',(0.21726221207405,0.258923021774215,0.4));
#35880=CARTESIAN_POINT('',(0.21726221207405,0.258923021774215,0.372));
#35881=CARTESIAN_POINT('',(0.221319030845725,0.27114182006011,0.36));
#35882=CARTESIAN_POINT('Ctrl Pts',(0.21726221207405,0.258923021774215,0.372));
#35883=CARTESIAN_POINT('Ctrl Pts',(0.219255242226414,0.264925861629787,
0.366120462798035));
#35884=CARTESIAN_POINT('Ctrl Pts',(0.221319030845725,0.27114182006011,0.36));
#35885=CARTESIAN_POINT('',(0.21726221207405,0.258923021774215,0.4));
#35886=CARTESIAN_POINT('',(0.221319030845725,0.27114182006011,0.18));
#35887=CARTESIAN_POINT('Origin',(0.265979360424374,0.285227943631476,0.4));
#35888=CARTESIAN_POINT('',(0.228590920171666,0.265039980408751,0.36));
#35889=CARTESIAN_POINT('Ctrl Pts',(0.228590920171666,0.265039980408751,
0.36));
#35890=CARTESIAN_POINT('Ctrl Pts',(0.222827769249913,0.261928155521995,
0.366120462798037));
#35891=CARTESIAN_POINT('Ctrl Pts',(0.21726221207405,0.258923021774215,0.372));
#35892=CARTESIAN_POINT('',(0.228590920171666,0.265039980408751,0.18));
#35893=CARTESIAN_POINT('Origin',(0.29271658647914,0.169,0.4));
#35894=CARTESIAN_POINT('',(0.29271658647914,0.169,0.372));
#35895=CARTESIAN_POINT('',(0.300707824283758,0.179094400846393,0.36));
#35896=CARTESIAN_POINT('Ctrl Pts',(0.29271658647914,0.169,0.372));
#35897=CARTESIAN_POINT('Ctrl Pts',(0.296642514354088,0.173959167857681,
0.366120462798029));
#35898=CARTESIAN_POINT('Ctrl Pts',(0.300707824283758,0.179094400846393,
0.36));
#35899=CARTESIAN_POINT('',(0.29271658647914,0.169,0.4));
#35900=CARTESIAN_POINT('',(0.300707824283758,0.179094400846393,0.18));
#35901=CARTESIAN_POINT('Origin',(0.347492544433463,0.177056294898423,0.4));
#35902=CARTESIAN_POINT('',(0.305454212950408,0.170873414523285,0.36));
#35903=CARTESIAN_POINT('Ctrl Pts',(0.305454212950408,0.170873414523285,
0.36));
#35904=CARTESIAN_POINT('Ctrl Pts',(0.298974315762989,0.169920369344288,
0.366120462798037));
#35905=CARTESIAN_POINT('Ctrl Pts',(0.29271658647914,0.169,0.372));
#35906=CARTESIAN_POINT('',(0.305454212950408,0.170873414523285,0.18));
#35907=CARTESIAN_POINT('Origin',(0.332865020518126,0.0586930840514224,0.4));
#35908=CARTESIAN_POINT('',(0.332865020518126,0.0586930840514225,0.372));
#35909=CARTESIAN_POINT('',(0.343826816138341,0.0654455537387478,0.36));
#35910=CARTESIAN_POINT('Ctrl Pts',(0.332865020518126,0.0586930840514225,
0.372));
#35911=CARTESIAN_POINT('Ctrl Pts',(0.338250321273409,0.0620104310780461,
0.366120462798033));
#35912=CARTESIAN_POINT('Ctrl Pts',(0.343826816138341,0.0654455537387478,
0.36));
#35913=CARTESIAN_POINT('',(0.332865020518126,0.0586930840514224,0.4));
#35914=CARTESIAN_POINT('',(0.343826816138341,0.0654455537387478,0.18));
#35915=CARTESIAN_POINT('Origin',(0.387092999140116,0.0475290439280075,0.4));
#35916=CARTESIAN_POINT('',(0.345475219623267,0.0560969930232949,0.36));
#35917=CARTESIAN_POINT('Ctrl Pts',(0.345475219623267,0.0560969930232949,
0.36));
#35918=CARTESIAN_POINT('Ctrl Pts',(0.339060147404081,0.0574176788660925,
0.366120462798036));
#35919=CARTESIAN_POINT('Ctrl Pts',(0.332865020518126,0.0586930840514225,
0.372));
#35920=CARTESIAN_POINT('',(0.345475219623267,0.0560969930232949,0.18));
#35921=CARTESIAN_POINT('Origin',(0.317616105825637,0.115602808444076,0.4));
#35922=CARTESIAN_POINT('',(0.317616105825637,0.115602808444076,0.372));
#35923=CARTESIAN_POINT('',(0.327238813083405,0.124156188777542,0.36));
#35924=CARTESIAN_POINT('Ctrl Pts',(0.317616105825637,0.115602808444076,
0.372));
#35925=CARTESIAN_POINT('Ctrl Pts',(0.322343540495878,0.119804905177669,
0.366120462798035));
#35926=CARTESIAN_POINT('Ctrl Pts',(0.327238813083405,0.124156188777542,
0.36));
#35927=CARTESIAN_POINT('',(0.317616105825637,0.115602808444076,0.4));
#35928=CARTESIAN_POINT('',(0.327238813083405,0.124156188777542,0.18));
#35929=CARTESIAN_POINT('Origin',(0.372958854825584,0.114024964841867,0.4));
#35930=CARTESIAN_POINT('',(0.330485534147499,0.115235895966675,0.36));
#35931=CARTESIAN_POINT('Ctrl Pts',(0.330485534147499,0.115235895966675,
0.36));
#35932=CARTESIAN_POINT('Ctrl Pts',(0.323938586600038,0.115422552023493,
0.366120462798038));
#35933=CARTESIAN_POINT('Ctrl Pts',(0.317616105825637,0.115602808444076,
0.372));
#35934=CARTESIAN_POINT('',(0.330485534147499,0.115235895966675,0.18));
#35935=CARTESIAN_POINT('Origin',(0.258923021774215,0.21726221207405,0.4));
#35936=CARTESIAN_POINT('',(0.258923021774215,0.21726221207405,0.372));
#35937=CARTESIAN_POINT('',(0.265039980408751,0.228590920171666,0.36));
#35938=CARTESIAN_POINT('Ctrl Pts',(0.258923021774215,0.21726221207405,0.372));
#35939=CARTESIAN_POINT('Ctrl Pts',(0.261928155521996,0.222827769249914,
0.366120462798035));
#35940=CARTESIAN_POINT('Ctrl Pts',(0.265039980408751,0.228590920171666,
0.36));
#35941=CARTESIAN_POINT('',(0.258923021774215,0.21726221207405,0.4));
#35942=CARTESIAN_POINT('',(0.265039980408751,0.228590920171666,0.18));
#35943=CARTESIAN_POINT('Origin',(0.311467848918444,0.234707859029299,0.4));
#35944=CARTESIAN_POINT('',(0.27114182006011,0.221319030845725,0.36));
#35945=CARTESIAN_POINT('Ctrl Pts',(0.27114182006011,0.221319030845725,0.36));
#35946=CARTESIAN_POINT('Ctrl Pts',(0.264925861629781,0.219255242226412,
0.36612046279804));
#35947=CARTESIAN_POINT('Ctrl Pts',(0.258923021774215,0.21726221207405,0.372));
#35948=CARTESIAN_POINT('',(0.27114182006011,0.221319030845725,0.18));
#35949=CARTESIAN_POINT('Origin',(0.169,0.29271658647914,0.4));
#35950=CARTESIAN_POINT('',(0.169,0.29271658647914,0.372));
#35951=CARTESIAN_POINT('',(0.170873414523285,0.305454212950408,0.36));
#35952=CARTESIAN_POINT('Ctrl Pts',(0.169,0.29271658647914,0.372));
#35953=CARTESIAN_POINT('Ctrl Pts',(0.169920369344288,0.298974315762989,
0.366120462798037));
#35954=CARTESIAN_POINT('Ctrl Pts',(0.170873414523285,0.305454212950408,
0.36));
#35955=CARTESIAN_POINT('',(0.169,0.29271658647914,0.4));
#35956=CARTESIAN_POINT('',(0.170873414523285,0.305454212950408,0.18));
#35957=CARTESIAN_POINT('Origin',(0.212409223655861,0.327081521498715,0.4));
#35958=CARTESIAN_POINT('',(0.179094400846393,0.300707824283758,0.36));
#35959=CARTESIAN_POINT('Ctrl Pts',(0.179094400846393,0.300707824283758,
0.36));
#35960=CARTESIAN_POINT('Ctrl Pts',(0.17395916785767,0.296642514354079,0.366120462798043));
#35961=CARTESIAN_POINT('Ctrl Pts',(0.169,0.29271658647914,0.372));
#35962=CARTESIAN_POINT('',(0.179094400846393,0.300707824283758,0.18));
#35963=CARTESIAN_POINT('Origin',(0.0586930840514225,0.332865020518126,0.4));
#35964=CARTESIAN_POINT('',(0.0586930840514225,0.332865020518126,0.372));
#35965=CARTESIAN_POINT('',(0.0560969930232949,0.345475219623267,0.36));
#35966=CARTESIAN_POINT('Ctrl Pts',(0.0586930840514225,0.332865020518126,
0.372));
#35967=CARTESIAN_POINT('Ctrl Pts',(0.0574176788660923,0.339060147404083,
0.366120462798035));
#35968=CARTESIAN_POINT('Ctrl Pts',(0.0560969930232949,0.345475219623267,
0.36));
#35969=CARTESIAN_POINT('',(0.0586930840514225,0.332865020518126,0.4));
#35970=CARTESIAN_POINT('',(0.0560969930232949,0.345475219623267,0.18));
#35971=CARTESIAN_POINT('Origin',(0.0877309111941073,0.380004325266242,0.4));
#35972=CARTESIAN_POINT('',(0.0654455537387478,0.343826816138341,0.36));
#35973=CARTESIAN_POINT('Ctrl Pts',(0.0654455537387477,0.343826816138341,
0.36));
#35974=CARTESIAN_POINT('Ctrl Pts',(0.0620104310780447,0.338250321273407,
0.366120462798036));
#35975=CARTESIAN_POINT('Ctrl Pts',(0.0586930840514225,0.332865020518126,
0.372));
#35976=CARTESIAN_POINT('',(0.0654455537387478,0.343826816138341,0.18));
#35977=CARTESIAN_POINT('Origin',(-0.0586930840514224,0.332865020518126,
0.4));
#35978=CARTESIAN_POINT('',(-0.0586930840514225,0.332865020518126,0.372));
#35979=CARTESIAN_POINT('',(-0.0654455537387477,0.343826816138341,0.36));
#35980=CARTESIAN_POINT('Ctrl Pts',(-0.0586930840514225,0.332865020518126,
0.372));
#35981=CARTESIAN_POINT('Ctrl Pts',(-0.0620104310780444,0.338250321273406,
0.366120462798036));
#35982=CARTESIAN_POINT('Ctrl Pts',(-0.0654455537387477,0.343826816138341,
0.36));
#35983=CARTESIAN_POINT('',(-0.0586930840514224,0.332865020518126,0.4));
#35984=CARTESIAN_POINT('',(-0.0654455537387477,0.343826816138341,0.18));
#35985=CARTESIAN_POINT('Origin',(-0.0475290439280075,0.387092999140116,
0.4));
#35986=CARTESIAN_POINT('',(-0.0560969930232949,0.345475219623267,0.36));
#35987=CARTESIAN_POINT('Ctrl Pts',(-0.0560969930232949,0.345475219623267,
0.36));
#35988=CARTESIAN_POINT('Ctrl Pts',(-0.0574176788660933,0.339060147404078,
0.36612046279804));
#35989=CARTESIAN_POINT('Ctrl Pts',(-0.0586930840514225,0.332865020518126,
0.372));
#35990=CARTESIAN_POINT('',(-0.0560969930232949,0.345475219623267,0.18));
#35991=CARTESIAN_POINT('Origin',(-0.169,0.29271658647914,0.4));
#35992=CARTESIAN_POINT('',(-0.169,0.29271658647914,0.372));
#35993=CARTESIAN_POINT('',(-0.179094400846393,0.300707824283758,0.36));
#35994=CARTESIAN_POINT('Ctrl Pts',(-0.169,0.29271658647914,0.372));
#35995=CARTESIAN_POINT('Ctrl Pts',(-0.173959167857679,0.296642514354086,
0.366120462798031));
#35996=CARTESIAN_POINT('Ctrl Pts',(-0.179094400846393,0.300707824283758,
0.36));
#35997=CARTESIAN_POINT('',(-0.169,0.29271658647914,0.4));
#35998=CARTESIAN_POINT('',(-0.179094400846393,0.300707824283758,0.18));
#35999=CARTESIAN_POINT('Origin',(-0.177056294898423,0.347492544433463,0.4));
#36000=CARTESIAN_POINT('',(-0.170873414523285,0.305454212950408,0.36));
#36001=CARTESIAN_POINT('Ctrl Pts',(-0.170873414523285,0.305454212950408,
0.36));
#36002=CARTESIAN_POINT('Ctrl Pts',(-0.169920369344288,0.29897431576299,
0.366120462798036));
#36003=CARTESIAN_POINT('Ctrl Pts',(-0.169,0.29271658647914,0.372));
#36004=CARTESIAN_POINT('',(-0.170873414523285,0.305454212950408,0.18));
#36005=CARTESIAN_POINT('Origin',(-0.258923021774215,0.21726221207405,0.4));
#36006=CARTESIAN_POINT('',(-0.258923021774215,0.21726221207405,0.372));
#36007=CARTESIAN_POINT('',(-0.27114182006011,0.221319030845725,0.36));
#36008=CARTESIAN_POINT('Ctrl Pts',(-0.258923021774215,0.21726221207405,
0.372));
#36009=CARTESIAN_POINT('Ctrl Pts',(-0.264925861629786,0.219255242226414,
0.366120462798035));
#36010=CARTESIAN_POINT('Ctrl Pts',(-0.27114182006011,0.221319030845725,
0.36));
#36011=CARTESIAN_POINT('',(-0.258923021774215,0.21726221207405,0.4));
#36012=CARTESIAN_POINT('',(-0.27114182006011,0.221319030845725,0.18));
#36013=CARTESIAN_POINT('Origin',(-0.285227943631476,0.265979360424374,0.4));
#36014=CARTESIAN_POINT('',(-0.265039980408751,0.228590920171666,0.36));
#36015=CARTESIAN_POINT('Ctrl Pts',(-0.265039980408751,0.228590920171666,
0.36));
#36016=CARTESIAN_POINT('Ctrl Pts',(-0.261928155521995,0.222827769249914,
0.366120462798036));
#36017=CARTESIAN_POINT('Ctrl Pts',(-0.258923021774215,0.21726221207405,
0.372));
#36018=CARTESIAN_POINT('',(-0.265039980408751,0.228590920171666,0.18));
#36019=CARTESIAN_POINT('Origin',(-0.317616105825637,0.115602808444076,0.4));
#36020=CARTESIAN_POINT('',(-0.317616105825637,0.115602808444076,0.372));
#36021=CARTESIAN_POINT('',(-0.330485534147499,0.115235895966675,0.36));
#36022=CARTESIAN_POINT('Ctrl Pts',(-0.317616105825637,0.115602808444076,
0.372));
#36023=CARTESIAN_POINT('Ctrl Pts',(-0.323938586600037,0.115422552023493,
0.366120462798039));
#36024=CARTESIAN_POINT('Ctrl Pts',(-0.330485534147499,0.115235895966675,
0.36));
#36025=CARTESIAN_POINT('',(-0.317616105825637,0.115602808444076,0.4));
#36026=CARTESIAN_POINT('',(-0.330485534147499,0.115235895966675,0.18));
#36027=CARTESIAN_POINT('Origin',(-0.358996892846452,0.152385140110817,0.4));
#36028=CARTESIAN_POINT('',(-0.327238813083405,0.124156188777542,0.36));
#36029=CARTESIAN_POINT('Ctrl Pts',(-0.327238813083405,0.124156188777542,
0.36));
#36030=CARTESIAN_POINT('Ctrl Pts',(-0.322343540495877,0.119804905177667,
0.366120462798037));
#36031=CARTESIAN_POINT('Ctrl Pts',(-0.317616105825637,0.115602808444076,
0.372));
#36032=CARTESIAN_POINT('',(-0.327238813083405,0.124156188777542,0.18));
#36033=CARTESIAN_POINT('Origin',(0.338,0.,0.4));
#36034=CARTESIAN_POINT('',(0.338,0.,0.372));
#36035=CARTESIAN_POINT('',(0.349967815369678,0.00474638866665024,0.36));
#36036=CARTESIAN_POINT('Ctrl Pts',(0.338,0.,0.372));
#36037=CARTESIAN_POINT('Ctrl Pts',(0.34387953720196,0.00233180140890496,
0.36612046279804));
#36038=CARTESIAN_POINT('Ctrl Pts',(0.349967815369678,0.00474638866665021,
0.36));
#36039=CARTESIAN_POINT('',(0.338,0.,0.4));
#36040=CARTESIAN_POINT('',(0.349967815369678,0.00474638866665024,0.18));
#36041=CARTESIAN_POINT('Origin',(0.389465518554284,-0.0204110229347481,
0.4));
#36042=CARTESIAN_POINT('',(0.349967815369678,-0.00474638866665023,0.36));
#36043=CARTESIAN_POINT('Ctrl Pts',(0.349967815369678,-0.00474638866665021,
0.36));
#36044=CARTESIAN_POINT('Ctrl Pts',(0.343879537201961,-0.00233180140890561,
0.366120462798039));
#36045=CARTESIAN_POINT('Ctrl Pts',(0.338,0.,0.372));
#36046=CARTESIAN_POINT('',(0.349967815369678,-0.00474638866665023,0.18));
#36047=CARTESIAN_POINT('Origin',(-0.332865020518126,-0.0586930840514225,
0.4));
#36048=CARTESIAN_POINT('',(-0.332865020518126,-0.0586930840514225,0.372));
#36049=CARTESIAN_POINT('',(-0.343826816138341,-0.0654455537387478,0.36));
#36050=CARTESIAN_POINT('Ctrl Pts',(-0.332865020518126,-0.0586930840514225,
0.372));
#36051=CARTESIAN_POINT('Ctrl Pts',(-0.338250321273407,-0.062010431078045,
0.366120462798035));
#36052=CARTESIAN_POINT('Ctrl Pts',(-0.343826816138341,-0.0654455537387477,
0.36));
#36053=CARTESIAN_POINT('',(-0.332865020518126,-0.0586930840514225,0.4));
#36054=CARTESIAN_POINT('',(-0.343826816138341,-0.0654455537387478,0.18));
#36055=CARTESIAN_POINT('Origin',(-0.387092999140116,-0.0475290439280074,
0.4));
#36056=CARTESIAN_POINT('',(-0.345475219623267,-0.0560969930232949,0.36));
#36057=CARTESIAN_POINT('Ctrl Pts',(-0.345475219623267,-0.0560969930232949,
0.36));
#36058=CARTESIAN_POINT('Ctrl Pts',(-0.339060147404077,-0.0574176788660935,
0.366120462798041));
#36059=CARTESIAN_POINT('Ctrl Pts',(-0.332865020518126,-0.0586930840514225,
0.372));
#36060=CARTESIAN_POINT('',(-0.345475219623267,-0.0560969930232949,0.18));
#36061=CARTESIAN_POINT('Origin',(-0.29271658647914,-0.169,0.4));
#36062=CARTESIAN_POINT('',(-0.29271658647914,-0.169,0.372));
#36063=CARTESIAN_POINT('',(-0.300707824283758,-0.179094400846393,0.36));
#36064=CARTESIAN_POINT('Ctrl Pts',(-0.29271658647914,-0.169,0.372));
#36065=CARTESIAN_POINT('Ctrl Pts',(-0.296642514354083,-0.173959167857676,
0.366120462798036));
#36066=CARTESIAN_POINT('Ctrl Pts',(-0.300707824283758,-0.179094400846393,
0.36));
#36067=CARTESIAN_POINT('',(-0.29271658647914,-0.169,0.4));
#36068=CARTESIAN_POINT('',(-0.300707824283758,-0.179094400846393,0.18));
#36069=CARTESIAN_POINT('Origin',(-0.347492544433463,-0.177056294898423,
0.4));
#36070=CARTESIAN_POINT('',(-0.305454212950408,-0.170873414523285,0.36));
#36071=CARTESIAN_POINT('Ctrl Pts',(-0.305454212950408,-0.170873414523285,
0.36));
#36072=CARTESIAN_POINT('Ctrl Pts',(-0.298974315762994,-0.169920369344289,
0.366120462798032));
#36073=CARTESIAN_POINT('Ctrl Pts',(-0.29271658647914,-0.169,0.372));
#36074=CARTESIAN_POINT('',(-0.305454212950408,-0.170873414523285,0.18));
#36075=CARTESIAN_POINT('Origin',(-0.21726221207405,-0.258923021774215,0.4));
#36076=CARTESIAN_POINT('',(-0.21726221207405,-0.258923021774215,0.372));
#36077=CARTESIAN_POINT('',(-0.221319030845725,-0.27114182006011,0.36));
#36078=CARTESIAN_POINT('Ctrl Pts',(-0.21726221207405,-0.258923021774215,
0.372));
#36079=CARTESIAN_POINT('Ctrl Pts',(-0.219255242226414,-0.264925861629784,
0.366120462798037));
#36080=CARTESIAN_POINT('Ctrl Pts',(-0.221319030845725,-0.27114182006011,
0.36));
#36081=CARTESIAN_POINT('',(-0.21726221207405,-0.258923021774215,0.4));
#36082=CARTESIAN_POINT('',(-0.221319030845725,-0.27114182006011,0.18));
#36083=CARTESIAN_POINT('Origin',(-0.265979360424374,-0.285227943631476,
0.4));
#36084=CARTESIAN_POINT('',(-0.228590920171666,-0.265039980408751,0.36));
#36085=CARTESIAN_POINT('Ctrl Pts',(-0.228590920171666,-0.265039980408751,
0.36));
#36086=CARTESIAN_POINT('Ctrl Pts',(-0.222827769249914,-0.261928155521995,
0.366120462798036));
#36087=CARTESIAN_POINT('Ctrl Pts',(-0.21726221207405,-0.258923021774215,
0.372));
#36088=CARTESIAN_POINT('',(-0.228590920171666,-0.265039980408751,0.18));
#36089=CARTESIAN_POINT('Origin',(-0.115602808444076,-0.317616105825637,
0.4));
#36090=CARTESIAN_POINT('',(-0.115602808444076,-0.317616105825637,0.372));
#36091=CARTESIAN_POINT('',(-0.115235895966675,-0.330485534147499,0.36));
#36092=CARTESIAN_POINT('Ctrl Pts',(-0.115602808444076,-0.317616105825637,
0.372));
#36093=CARTESIAN_POINT('Ctrl Pts',(-0.115422552023493,-0.323938586600039,
0.366120462798037));
#36094=CARTESIAN_POINT('Ctrl Pts',(-0.115235895966675,-0.330485534147499,
0.36));
#36095=CARTESIAN_POINT('',(-0.115602808444076,-0.317616105825637,0.4));
#36096=CARTESIAN_POINT('',(-0.115235895966675,-0.330485534147499,0.18));
#36097=CARTESIAN_POINT('Origin',(-0.152385140110817,-0.358996892846452,
0.4));
#36098=CARTESIAN_POINT('',(-0.124156188777542,-0.327238813083405,0.36));
#36099=CARTESIAN_POINT('Ctrl Pts',(-0.124156188777541,-0.327238813083405,
0.36));
#36100=CARTESIAN_POINT('Ctrl Pts',(-0.119804905177672,-0.322343540495882,
0.366120462798031));
#36101=CARTESIAN_POINT('Ctrl Pts',(-0.115602808444076,-0.317616105825637,
0.372));
#36102=CARTESIAN_POINT('',(-0.124156188777542,-0.327238813083405,0.18));
#36103=CARTESIAN_POINT('Origin',(-6.20895927167708E-17,-0.338,0.4));
#36104=CARTESIAN_POINT('',(-6.20895927167708E-17,-0.338,0.372));
#36105=CARTESIAN_POINT('',(0.00474638866665021,-0.349967815369678,0.36));
#36106=CARTESIAN_POINT('Ctrl Pts',(-6.20895927167708E-17,-0.338,0.372));
#36107=CARTESIAN_POINT('Ctrl Pts',(0.00233180140890712,-0.343879537201965,
0.366120462798035));
#36108=CARTESIAN_POINT('Ctrl Pts',(0.00474638866665021,-0.349967815369678,
0.36));
#36109=CARTESIAN_POINT('',(-6.20895927167708E-17,-0.338,0.4));
#36110=CARTESIAN_POINT('',(0.00474638866665021,-0.349967815369678,0.18));
#36111=CARTESIAN_POINT('Origin',(-0.0204110229347483,-0.389465518554284,
0.4));
#36112=CARTESIAN_POINT('',(-0.00474638866665032,-0.349967815369678,0.36));
#36113=CARTESIAN_POINT('Ctrl Pts',(-0.00474638866665031,-0.349967815369678,
0.36));
#36114=CARTESIAN_POINT('Ctrl Pts',(-0.00233180140890634,-0.343879537201963,
0.366120462798037));
#36115=CARTESIAN_POINT('Ctrl Pts',(-6.20895927167708E-17,-0.338,0.372));
#36116=CARTESIAN_POINT('',(-0.00474638866665032,-0.349967815369678,0.18));
#36117=CARTESIAN_POINT('Origin',(0.115602808444076,-0.317616105825637,0.4));
#36118=CARTESIAN_POINT('',(0.115602808444076,-0.317616105825637,0.372));
#36119=CARTESIAN_POINT('',(0.124156188777542,-0.327238813083405,0.36));
#36120=CARTESIAN_POINT('Ctrl Pts',(0.115602808444076,-0.317616105825637,
0.372));
#36121=CARTESIAN_POINT('Ctrl Pts',(0.119804905177668,-0.322343540495877,
0.366120462798037));
#36122=CARTESIAN_POINT('Ctrl Pts',(0.124156188777542,-0.327238813083405,
0.36));
#36123=CARTESIAN_POINT('',(0.115602808444076,-0.317616105825637,0.4));
#36124=CARTESIAN_POINT('',(0.124156188777542,-0.327238813083405,0.18));
#36125=CARTESIAN_POINT('Origin',(0.114024964841867,-0.372958854825584,0.4));
#36126=CARTESIAN_POINT('',(0.115235895966675,-0.330485534147499,0.36));
#36127=CARTESIAN_POINT('Ctrl Pts',(0.115235895966675,-0.330485534147499,
0.36));
#36128=CARTESIAN_POINT('Ctrl Pts',(0.115422552023493,-0.323938586600039,
0.366120462798037));
#36129=CARTESIAN_POINT('Ctrl Pts',(0.115602808444076,-0.317616105825637,
0.372));
#36130=CARTESIAN_POINT('',(0.115235895966675,-0.330485534147499,0.18));
#36131=CARTESIAN_POINT('Origin',(0.21726221207405,-0.258923021774215,0.4));
#36132=CARTESIAN_POINT('',(0.21726221207405,-0.258923021774215,0.372));
#36133=CARTESIAN_POINT('',(0.228590920171666,-0.265039980408751,0.36));
#36134=CARTESIAN_POINT('Ctrl Pts',(0.21726221207405,-0.258923021774215,
0.372));
#36135=CARTESIAN_POINT('Ctrl Pts',(0.22282776924991,-0.261928155521994,
0.366120462798039));
#36136=CARTESIAN_POINT('Ctrl Pts',(0.228590920171666,-0.265039980408751,
0.36));
#36137=CARTESIAN_POINT('',(0.21726221207405,-0.258923021774215,0.4));
#36138=CARTESIAN_POINT('',(0.228590920171666,-0.265039980408751,0.18));
#36139=CARTESIAN_POINT('Origin',(0.234707859029299,-0.311467848918444,0.4));
#36140=CARTESIAN_POINT('',(0.221319030845725,-0.27114182006011,0.36));
#36141=CARTESIAN_POINT('Ctrl Pts',(0.221319030845725,-0.27114182006011,
0.36));
#36142=CARTESIAN_POINT('Ctrl Pts',(0.219255242226415,-0.264925861629789,
0.366120462798033));
#36143=CARTESIAN_POINT('Ctrl Pts',(0.21726221207405,-0.258923021774215,
0.372));
#36144=CARTESIAN_POINT('',(0.221319030845725,-0.27114182006011,0.18));
#36145=CARTESIAN_POINT('Origin',(0.29271658647914,-0.169,0.4));
#36146=CARTESIAN_POINT('',(0.29271658647914,-0.169,0.372));
#36147=CARTESIAN_POINT('',(0.305454212950408,-0.170873414523286,0.36));
#36148=CARTESIAN_POINT('Ctrl Pts',(0.29271658647914,-0.169,0.372));
#36149=CARTESIAN_POINT('Ctrl Pts',(0.298974315762989,-0.169920369344288,
0.366120462798037));
#36150=CARTESIAN_POINT('Ctrl Pts',(0.305454212950408,-0.170873414523285,
0.36));
#36151=CARTESIAN_POINT('',(0.29271658647914,-0.169,0.4));
#36152=CARTESIAN_POINT('',(0.305454212950408,-0.170873414523286,0.18));
#36153=CARTESIAN_POINT('Origin',(0.327081521498715,-0.212409223655861,0.4));
#36154=CARTESIAN_POINT('',(0.300707824283758,-0.179094400846393,0.36));
#36155=CARTESIAN_POINT('Ctrl Pts',(0.300707824283758,-0.179094400846393,
0.36));
#36156=CARTESIAN_POINT('Ctrl Pts',(0.296642514354083,-0.173959167857676,
0.366120462798036));
#36157=CARTESIAN_POINT('Ctrl Pts',(0.29271658647914,-0.169,0.372));
#36158=CARTESIAN_POINT('',(0.300707824283758,-0.179094400846393,0.18));
#36159=CARTESIAN_POINT('Origin',(0.332865020518126,-0.0586930840514225,
0.4));
#36160=CARTESIAN_POINT('',(0.332865020518126,-0.0586930840514225,0.372));
#36161=CARTESIAN_POINT('',(0.345475219623267,-0.0560969930232949,0.36));
#36162=CARTESIAN_POINT('Ctrl Pts',(0.332865020518126,-0.0586930840514225,
0.372));
#36163=CARTESIAN_POINT('Ctrl Pts',(0.339060147404081,-0.0574176788660926,
0.366120462798037));
#36164=CARTESIAN_POINT('Ctrl Pts',(0.345475219623267,-0.0560969930232949,
0.36));
#36165=CARTESIAN_POINT('',(0.332865020518126,-0.0586930840514225,0.4));
#36166=CARTESIAN_POINT('',(0.345475219623267,-0.0560969930232949,0.18));
#36167=CARTESIAN_POINT('Origin',(0.380004325266242,-0.0877309111941075,
0.4));
#36168=CARTESIAN_POINT('',(0.343826816138341,-0.0654455537387478,0.36));
#36169=CARTESIAN_POINT('Ctrl Pts',(0.343826816138341,-0.0654455537387478,
0.36));
#36170=CARTESIAN_POINT('Ctrl Pts',(0.338250321273404,-0.062010431078043,
0.366120462798039));
#36171=CARTESIAN_POINT('Ctrl Pts',(0.332865020518126,-0.0586930840514225,
0.372));
#36172=CARTESIAN_POINT('',(0.343826816138341,-0.0654455537387478,0.18));
#36173=CARTESIAN_POINT('Origin',(0.,0.,0.18));
#36174=CARTESIAN_POINT('Origin',(0.,0.,0.36));
#36175=CARTESIAN_POINT('Origin',(0.,0.,0.18));
#36176=CARTESIAN_POINT('Origin',(0.,0.,0.36));
#36177=CARTESIAN_POINT('Origin',(0.,0.,0.18));
#36178=CARTESIAN_POINT('Origin',(0.,0.,0.36));
#36179=CARTESIAN_POINT('Origin',(0.,0.,0.18));
#36180=CARTESIAN_POINT('Origin',(0.,0.,0.36));
#36181=CARTESIAN_POINT('Origin',(0.,0.,0.18));
#36182=CARTESIAN_POINT('Origin',(0.,0.,0.36));
#36183=CARTESIAN_POINT('Origin',(0.,0.,0.18));
#36184=CARTESIAN_POINT('Origin',(0.,0.,0.36));
#36185=CARTESIAN_POINT('Origin',(0.,0.,0.18));
#36186=CARTESIAN_POINT('Origin',(0.,0.,0.36));
#36187=CARTESIAN_POINT('Origin',(0.,0.,0.18));
#36188=CARTESIAN_POINT('Origin',(0.,0.,0.36));
#36189=CARTESIAN_POINT('Origin',(0.,0.,0.18));
#36190=CARTESIAN_POINT('Origin',(0.,0.,0.36));
#36191=CARTESIAN_POINT('Origin',(0.,0.,0.18));
#36192=CARTESIAN_POINT('Origin',(0.,0.,0.36));
#36193=CARTESIAN_POINT('Origin',(0.,0.,0.18));
#36194=CARTESIAN_POINT('Origin',(0.,0.,0.36));
#36195=CARTESIAN_POINT('Origin',(0.,0.,0.18));
#36196=CARTESIAN_POINT('Origin',(0.,0.,0.36));
#36197=CARTESIAN_POINT('Origin',(0.,0.,0.18));
#36198=CARTESIAN_POINT('Origin',(0.,0.,0.36));
#36199=CARTESIAN_POINT('Origin',(0.,0.,0.18));
#36200=CARTESIAN_POINT('Origin',(0.,0.,0.36));
#36201=CARTESIAN_POINT('Origin',(0.,0.,0.18));
#36202=CARTESIAN_POINT('Origin',(0.,0.,0.36));
#36203=CARTESIAN_POINT('Origin',(0.,0.,0.18));
#36204=CARTESIAN_POINT('Origin',(0.,0.,0.36));
#36205=CARTESIAN_POINT('Origin',(0.,0.,0.18));
#36206=CARTESIAN_POINT('Origin',(0.,0.,0.36));
#36207=CARTESIAN_POINT('Origin',(0.,0.,0.18));
#36208=CARTESIAN_POINT('Origin',(0.,0.,0.36));
#36209=CARTESIAN_POINT('Origin',(0.,0.,0.18));
#36210=CARTESIAN_POINT('Origin',(0.,0.,0.36));
#36211=CARTESIAN_POINT('Origin',(0.,0.,0.18));
#36212=CARTESIAN_POINT('Origin',(0.,0.,0.36));
#36213=CARTESIAN_POINT('Origin',(0.,0.,0.18));
#36214=CARTESIAN_POINT('Origin',(0.,0.,0.36));
#36215=CARTESIAN_POINT('Origin',(0.,0.,0.18));
#36216=CARTESIAN_POINT('Origin',(0.,0.,0.36));
#36217=CARTESIAN_POINT('Origin',(0.,0.,0.18));
#36218=CARTESIAN_POINT('Origin',(0.,0.,0.36));
#36219=CARTESIAN_POINT('Origin',(0.,0.,0.18));
#36220=CARTESIAN_POINT('Origin',(0.,0.,0.36));
#36221=CARTESIAN_POINT('Origin',(0.,0.,0.18));
#36222=CARTESIAN_POINT('Origin',(0.,0.,0.36));
#36223=CARTESIAN_POINT('Origin',(0.,0.,0.18));
#36224=CARTESIAN_POINT('Origin',(0.,0.,0.36));
#36225=CARTESIAN_POINT('Origin',(0.,0.,0.18));
#36226=CARTESIAN_POINT('Origin',(0.,0.,0.36));
#36227=CARTESIAN_POINT('Origin',(0.,0.,0.18));
#36228=CARTESIAN_POINT('Origin',(0.,0.,0.36));
#36229=CARTESIAN_POINT('Origin',(0.,0.,0.18));
#36230=CARTESIAN_POINT('Origin',(0.,0.,0.36));
#36231=CARTESIAN_POINT('Origin',(0.,0.,0.18));
#36232=CARTESIAN_POINT('Origin',(0.,0.,0.36));
#36233=CARTESIAN_POINT('Origin',(0.,0.,0.18));
#36234=CARTESIAN_POINT('Origin',(0.,0.,0.36));
#36235=CARTESIAN_POINT('Origin',(0.,0.,0.18));
#36236=CARTESIAN_POINT('Origin',(0.,0.,0.36));
#36237=CARTESIAN_POINT('Origin',(0.,0.,0.18));
#36238=CARTESIAN_POINT('Origin',(0.,0.,0.36));
#36239=CARTESIAN_POINT('Origin',(0.,0.,0.18));
#36240=CARTESIAN_POINT('Origin',(0.,0.,0.36));
#36241=CARTESIAN_POINT('Origin',(0.,0.,0.18));
#36242=CARTESIAN_POINT('Origin',(0.,0.,0.36));
#36243=CARTESIAN_POINT('Origin',(0.,0.,0.18));
#36244=CARTESIAN_POINT('Origin',(0.,0.,0.36));
#36245=CARTESIAN_POINT('Origin',(0.16,0.,-1.6));
#36246=CARTESIAN_POINT('',(-0.16,-1.95943487863577E-17,-1.6));
#36247=CARTESIAN_POINT('Origin',(0.,0.,-1.6));
#36248=CARTESIAN_POINT('Origin',(0.,0.,-1.58));
#36249=CARTESIAN_POINT('',(-0.18,-2.20436423846524E-17,-1.58));
#36250=CARTESIAN_POINT('Origin',(0.,0.,0.38));
#36251=CARTESIAN_POINT('',(-0.31,-3.7964050773568E-17,0.4));
#36252=CARTESIAN_POINT('Origin',(0.,0.,0.4));
#36253=CARTESIAN_POINT('',(-0.33,-4.04133443718627E-17,0.38));
#36254=CARTESIAN_POINT('Origin',(0.,0.,0.4));
#36255=CARTESIAN_POINT('',(0.,0.,0.));
#36256=CARTESIAN_POINT('Origin',(0.,0.,-0.385));
#36257=CARTESIAN_POINT('',(-0.195612035850383,0.000135947154934524,-0.752013030787577));
#36258=CARTESIAN_POINT('',(-0.195578202233822,0.00020702102411161,-0.762186969212424));
#36259=CARTESIAN_POINT('',(-0.1954,-2.39295984553393E-17,-0.385));
#36260=CARTESIAN_POINT('',(0.0862546024668518,0.17550570910154,-0.7746));
#36261=CARTESIAN_POINT('Ctrl Pts',(-0.195612035850383,0.000135947154934524,
-0.752013030787577));
#36262=CARTESIAN_POINT('Ctrl Pts',(-0.195667083286635,0.00761212544448936,
-0.752440649041024));
#36263=CARTESIAN_POINT('Ctrl Pts',(-0.19527544420465,0.0150821391217423,
-0.752868267294471));
#36264=CARTESIAN_POINT('Ctrl Pts',(-0.194417810721063,0.0224978227107708,
-0.753295885547918));
#36265=CARTESIAN_POINT('Ctrl Pts',(-0.187011858244344,0.0865347350909431,
-0.756988512437858));
#36266=CARTESIAN_POINT('Ctrl Pts',(-0.144857163949201,0.146520306506109,
-0.760681139327799));
#36267=CARTESIAN_POINT('Ctrl Pts',(-0.0871192266947845,0.175237646686046,
-0.76437376621774));
#36268=CARTESIAN_POINT('Ctrl Pts',(-0.0338200748021689,0.201747251098443,
-0.767782510811827));
#36269=CARTESIAN_POINT('Ctrl Pts',(0.0327583993499999,0.201611508316804,
-0.771191255405914));
#36270=CARTESIAN_POINT('Ctrl Pts',(0.0863566189666486,0.175629287040327,
-0.7746));
#36271=CARTESIAN_POINT('',(-0.0861525859670513,0.175382131162755,-0.7746));
#36272=CARTESIAN_POINT('Origin',(0.,0.,-0.7746));
#36273=CARTESIAN_POINT('Ctrl Pts',(-0.0861525859670512,0.175382131162755,
-0.7746));
#36274=CARTESIAN_POINT('Ctrl Pts',(-0.144282890666664,0.146826906980442,
-0.770907373110059));
#36275=CARTESIAN_POINT('Ctrl Pts',(-0.186613134667349,0.0873604776073136,
-0.767214746220119));
#36276=CARTESIAN_POINT('Ctrl Pts',(-0.194290909418724,0.023452807632156,
-0.763522119330178));
#36277=CARTESIAN_POINT('Ctrl Pts',(-0.195216265284969,0.0157504017626666,
-0.763077069290927));
#36278=CARTESIAN_POINT('Ctrl Pts',(-0.195638258465322,0.00798348231459053,
-0.762632019251675));
#36279=CARTESIAN_POINT('Ctrl Pts',(-0.195578202233822,0.00020702102411161,
-0.762186969212424));
#36280=CARTESIAN_POINT('Origin',(0.,0.,-0.385));
#36281=CARTESIAN_POINT('',(-0.195106158228715,6.7253471116302E-5,-0.682013030787577));
#36282=CARTESIAN_POINT('',(-0.195102641109175,6.37944958194417E-5,-0.692186969212424));
#36283=CARTESIAN_POINT('',(-0.1954,-2.39295984553393E-17,-0.385));
#36284=CARTESIAN_POINT('Ctrl Pts',(-0.195106158228715,6.7253471116302E-5,
-0.682013030787577));
#36285=CARTESIAN_POINT('Ctrl Pts',(-0.195193741697796,0.0283198531480969,
-0.683618221034713));
#36286=CARTESIAN_POINT('Ctrl Pts',(-0.18945610577258,0.0565385117234044,
-0.685223411281848));
#36287=CARTESIAN_POINT('Ctrl Pts',(-0.177715395582584,0.0819875737941825,
-0.686828601528984));
#36288=CARTESIAN_POINT('Ctrl Pts',(-0.150706720298178,0.140531345221913,
-0.690521228418925));
#36289=CARTESIAN_POINT('Ctrl Pts',(-0.0919299226246749,0.184418479592776,
-0.694213855308865));
#36290=CARTESIAN_POINT('Ctrl Pts',(-0.0281252717103119,0.19368402419514,
-0.697906482198806));
#36291=CARTESIAN_POINT('Ctrl Pts',(0.0356793792040508,0.202949568797503,
-0.701599109088747));
#36292=CARTESIAN_POINT('Ctrl Pts',(0.104511883359273,0.177593523631367,
-0.705291735978687));
#36293=CARTESIAN_POINT('Ctrl Pts',(0.147056344142496,0.129148732777355,
-0.708984362868628));
#36294=CARTESIAN_POINT('Ctrl Pts',(0.189600804925718,0.080703941923342,
-0.712676989758569));
#36295=CARTESIAN_POINT('Ctrl Pts',(0.20585722233694,0.00917040538145272,
-0.71636961664851));
#36296=CARTESIAN_POINT('Ctrl Pts',(0.1884307024384,-0.0529021236960677,
-0.720062243538451));
#36297=CARTESIAN_POINT('Ctrl Pts',(0.171004182539859,-0.114974652773588,
-0.723754870428392));
#36298=CARTESIAN_POINT('Ctrl Pts',(0.119894725331557,-0.16758617438674,
-0.727447497318332));
#36299=CARTESIAN_POINT('Ctrl Pts',(0.0583527546211337,-0.186811585253294,
-0.731140124208273));
#36300=CARTESIAN_POINT('Ctrl Pts',(-0.00318921608928925,-0.206036996119848,
-0.734832751098214));
#36301=CARTESIAN_POINT('Ctrl Pts',(-0.0751637003018327,-0.191876296239803,
-0.738525377988155));
#36302=CARTESIAN_POINT('Ctrl Pts',(-0.124822337078956,-0.150751819627192,
-0.742218004878095));
#36303=CARTESIAN_POINT('Ctrl Pts',(-0.168730341539278,-0.114389691712985,
-0.745483013514589));
#36304=CARTESIAN_POINT('Ctrl Pts',(-0.195191730231224,-0.0569471789431846,
-0.748748022151083));
#36305=CARTESIAN_POINT('Ctrl Pts',(-0.195612035850383,0.000135947154934524,
-0.752013030787577));
#36306=CARTESIAN_POINT('Ctrl Pts',(-0.195578202233822,0.00020702102411161,
-0.762186969212424));
#36307=CARTESIAN_POINT('Ctrl Pts',(-0.195139965608823,-0.056538633261677,
-0.758939392361734));
#36308=CARTESIAN_POINT('Ctrl Pts',(-0.1690336868213,-0.113792369099031,
-0.755691815511045));
#36309=CARTESIAN_POINT('Ctrl Pts',(-0.125540731300798,-0.150194679039488,
-0.752444238660355));
#36310=CARTESIAN_POINT('Ctrl Pts',(-0.0760874729294314,-0.191585585158787,
-0.748751611770415));
#36311=CARTESIAN_POINT('Ctrl Pts',(-0.00415565068463411,-0.206018486820197,
-0.745058984880474));
#36312=CARTESIAN_POINT('Ctrl Pts',(0.0574817652959297,-0.187066360843203,
-0.741366357990533));
#36313=CARTESIAN_POINT('Ctrl Pts',(0.119119181276493,-0.168114234866209,
-0.737673731100593));
#36314=CARTESIAN_POINT('Ctrl Pts',(0.170462190992824,-0.11577708125081,
-0.733981104210652));
#36315=CARTESIAN_POINT('Ctrl Pts',(0.188176832473196,-0.0537951148800162,
-0.730288477320711));
#36316=CARTESIAN_POINT('Ctrl Pts',(0.205891473953568,0.00818685149077737,
-0.72659585043077));
#36317=CARTESIAN_POINT('Ctrl Pts',(0.189977747197981,0.0798136306169658,
-0.722903223540829));
#36318=CARTESIAN_POINT('Ctrl Pts',(0.147662757203391,0.128461801942711,
-0.719210596650889));
#36319=CARTESIAN_POINT('Ctrl Pts',(0.1053477672088,0.177109973268457,-0.715517969760948));
#36320=CARTESIAN_POINT('Ctrl Pts',(0.036631513975206,0.202779536793759,
-0.711825342871007));
#36321=CARTESIAN_POINT('Ctrl Pts',(-0.0272167615306242,0.193811384880893,
-0.708132715981067));
#36322=CARTESIAN_POINT('Ctrl Pts',(-0.0910650370364544,0.184843232968026,
-0.704440089091126));
#36323=CARTESIAN_POINT('Ctrl Pts',(-0.150045334814521,0.14123736561699,
-0.700747462201185));
#36324=CARTESIAN_POINT('Ctrl Pts',(-0.177328074880872,0.0828221813027525,
-0.697054835311244));
#36325=CARTESIAN_POINT('Ctrl Pts',(-0.189316715073911,0.0571532556431493,
-0.695432213278304));
#36326=CARTESIAN_POINT('Ctrl Pts',(-0.195184816078502,0.028624771980631,
-0.693809591245364));
#36327=CARTESIAN_POINT('Ctrl Pts',(-0.195102641109175,6.37944958194417E-5,
-0.692186969212424));
#36328=CARTESIAN_POINT('Origin',(0.,0.,-0.385));
#36329=CARTESIAN_POINT('',(-0.195373814288334,-0.000175590164213202,-0.612013030787577));
#36330=CARTESIAN_POINT('',(-0.195382883542994,-0.000175680656981076,-0.622186969212423));
#36331=CARTESIAN_POINT('',(-0.1954,-2.39295984553393E-17,-0.385));
#36332=CARTESIAN_POINT('Ctrl Pts',(-0.195373814288334,-0.000175590164213202,
-0.612013030787577));
#36333=CARTESIAN_POINT('Ctrl Pts',(-0.194935462027994,0.0486337685077184,
-0.614795793028401));
#36334=CARTESIAN_POINT('Ctrl Pts',(-0.176386685151872,0.0977403470970804,
-0.617578555269226));
#36335=CARTESIAN_POINT('Ctrl Pts',(-0.143291075940014,0.133313048722114,
-0.62036131751005));
#36336=CARTESIAN_POINT('Ctrl Pts',(-0.0993743752166056,0.180516763305194,
-0.624053944399991));
#36337=CARTESIAN_POINT('Ctrl Pts',(-0.0298431035570151,0.203889554183137,
-0.627746571289932));
#36338=CARTESIAN_POINT('Ctrl Pts',(0.0336694536774745,0.192797988921239,
-0.631439198179872));
#36339=CARTESIAN_POINT('Ctrl Pts',(0.0971820109119643,0.181706423659341,
-0.635131825069813));
#36340=CARTESIAN_POINT('Ctrl Pts',(0.154675853721353,0.136150502257601,
-0.638824451959754));
#36341=CARTESIAN_POINT('Ctrl Pts',(0.179994115466673,0.0768558559611854,
-0.642517078849694));
#36342=CARTESIAN_POINT('Ctrl Pts',(0.205312377211992,0.0175612096647699,
-0.646209705739635));
#36343=CARTESIAN_POINT('Ctrl Pts',(0.198455057893242,-0.0554721615263214,
-0.649902332629576));
#36344=CARTESIAN_POINT('Ctrl Pts',(0.162541919102326,-0.109017568867995,
-0.653594959519517));
#36345=CARTESIAN_POINT('Ctrl Pts',(0.12662878031141,-0.162562976209668,
-0.657287586409458));
#36346=CARTESIAN_POINT('Ctrl Pts',(0.0616598220483278,-0.196620419701923,
-0.660980213299398));
#36347=CARTESIAN_POINT('Ctrl Pts',(-0.00280733049035602,-0.195695666682811,
-0.664672840189339));
#36348=CARTESIAN_POINT('Ctrl Pts',(-0.0672744830290399,-0.194770913663699,
-0.66836546707928));
#36349=CARTESIAN_POINT('Ctrl Pts',(-0.131239829843325,-0.15886396413322,
-0.67205809396922));
#36350=CARTESIAN_POINT('Ctrl Pts',(-0.165602226802813,-0.104310285125682,
-0.675750720859161));
#36351=CARTESIAN_POINT('Ctrl Pts',(-0.185027240129573,-0.073471169245769,
-0.677838157501967));
#36352=CARTESIAN_POINT('Ctrl Pts',(-0.194992262107684,-0.0366732587052289,
-0.679925594144772));
#36353=CARTESIAN_POINT('Ctrl Pts',(-0.195106158228715,6.7253471116302E-5,
-0.682013030787577));
#36354=CARTESIAN_POINT('Ctrl Pts',(-0.195102641109175,6.37944958194417E-5,
-0.692186969212424));
#36355=CARTESIAN_POINT('Ctrl Pts',(-0.194997809187644,-0.0363719008873622,
-0.690116964355423));
#36356=CARTESIAN_POINT('Ctrl Pts',(-0.185209193124591,-0.0728604783826336,
-0.688046959498422));
#36357=CARTESIAN_POINT('Ctrl Pts',(-0.166090287545791,-0.103532484641873,
-0.685976954641422));
#36358=CARTESIAN_POINT('Ctrl Pts',(-0.131984577789722,-0.158247464994821,
-0.682284327751481));
#36359=CARTESIAN_POINT('Ctrl Pts',(-0.0681879759229486,-0.194452924423278,
-0.67859170086154));
#36360=CARTESIAN_POINT('Ctrl Pts',(-0.00372575719310086,-0.195679956595876,
-0.674899073971599));
#36361=CARTESIAN_POINT('Ctrl Pts',(0.060736461536747,-0.196906988768474,
-0.671206447081658));
#36362=CARTESIAN_POINT('Ctrl Pts',(0.125864297129669,-0.163155593685212,
-0.667513820191718));
#36363=CARTESIAN_POINT('Ctrl Pts',(0.162028316469382,-0.109779523904799,
-0.663821193301777));
#36364=CARTESIAN_POINT('Ctrl Pts',(0.198192335809096,-0.0564034541243863,
-0.660128566411836));
#36365=CARTESIAN_POINT('Ctrl Pts',(0.205392538895601,0.0165972903531772,
-0.656435939521895));
#36366=CARTESIAN_POINT('Ctrl Pts',(0.180352920431713,0.0760102116200135,
-0.652743312631955));
#36367=CARTESIAN_POINT('Ctrl Pts',(0.155313301967824,0.13542313288685,-0.649050685742014));
#36368=CARTESIAN_POINT('Ctrl Pts',(0.0980338619535436,0.181248230942959,
-0.645358058852073));
#36369=CARTESIAN_POINT('Ctrl Pts',(0.0345740548428563,0.19263775515523,
-0.641665431962132));
#36370=CARTESIAN_POINT('Ctrl Pts',(-0.028885752267831,0.2040272793675,-0.637972805072192));
#36371=CARTESIAN_POINT('Ctrl Pts',(-0.0985259264749248,0.180981229735933,
-0.634280178182251));
#36372=CARTESIAN_POINT('Ctrl Pts',(-0.142663705648477,0.133984207668471,
-0.63058755129231));
#36373=CARTESIAN_POINT('Ctrl Pts',(-0.176134280736128,0.0983454105776664,
-0.627787357265681));
#36374=CARTESIAN_POINT('Ctrl Pts',(-0.194939710785028,0.0489336135733413,
-0.624987163239052));
#36375=CARTESIAN_POINT('Ctrl Pts',(-0.195382883542994,-0.000175680656981076,
-0.622186969212423));
#36376=CARTESIAN_POINT('Origin',(0.,0.,-0.385));
#36377=CARTESIAN_POINT('',(-0.195672562949621,8.22112365601695E-5,-0.542013030787577));
#36378=CARTESIAN_POINT('',(-0.195667167474188,8.703216064893E-5,-0.552186969212423));
#36379=CARTESIAN_POINT('',(-0.1954,-2.39295984553393E-17,-0.385));
#36380=CARTESIAN_POINT('Ctrl Pts',(-0.195672562949621,8.22112365601695E-5,
-0.542013030787577));
#36381=CARTESIAN_POINT('Ctrl Pts',(-0.195697468556697,0.00475918250908728,
-0.542280738132149));
#36382=CARTESIAN_POINT('Ctrl Pts',(-0.195544212090925,0.00943449414701473,
-0.542548445476721));
#36383=CARTESIAN_POINT('Ctrl Pts',(-0.195207549301115,0.0140965614284866,
-0.542816152821294));
#36384=CARTESIAN_POINT('Ctrl Pts',(-0.190563784026466,0.0784028845657411,
-0.546508779711234));
#36385=CARTESIAN_POINT('Ctrl Pts',(-0.151024907292751,0.140189320250109,
-0.550201406601176));
#36386=CARTESIAN_POINT('Ctrl Pts',(-0.0945791532634838,0.171346094632147,
-0.553894033491116));
#36387=CARTESIAN_POINT('Ctrl Pts',(-0.0381333992342172,0.202502869014184,
-0.557586660381057));
#36388=CARTESIAN_POINT('Ctrl Pts',(0.0352192320906011,0.20302998209389,
-0.561279287270997));
#36389=CARTESIAN_POINT('Ctrl Pts',(0.0921069201474241,0.172687624146735,
-0.564971914160938));
#36390=CARTESIAN_POINT('Ctrl Pts',(0.148994608204248,0.142345266199579,
-0.568664541050879));
#36391=CARTESIAN_POINT('Ctrl Pts',(0.189417352993076,0.0811334372255617,
-0.57235716794082));
#36392=CARTESIAN_POINT('Ctrl Pts',(0.194984803922326,0.0169004918108476,
-0.576049794830761));
#36393=CARTESIAN_POINT('Ctrl Pts',(0.200552254851577,-0.0473324536038658,
-0.579742421720702));
#36394=CARTESIAN_POINT('Ctrl Pts',(0.171264411921251,-0.114586515459276,
-0.583435048610642));
#36395=CARTESIAN_POINT('Ctrl Pts',(0.120445796091562,-0.154264418250576,
-0.587127675500583));
#36396=CARTESIAN_POINT('Ctrl Pts',(0.0696271802618727,-0.193942321041876,
-0.590820302390524));
#36397=CARTESIAN_POINT('Ctrl Pts',(-0.00272220846717902,-0.206044064769067,
-0.594512929280465));
#36398=CARTESIAN_POINT('Ctrl Pts',(-0.0636869760053119,-0.185063958956186,
-0.598205556170405));
#36399=CARTESIAN_POINT('Ctrl Pts',(-0.124651743543445,-0.164083853143304,
-0.601898183060346));
#36400=CARTESIAN_POINT('Ctrl Pts',(-0.174231889890659,-0.110021897790351,
-0.605590809950287));
#36401=CARTESIAN_POINT('Ctrl Pts',(-0.189870898170653,-0.0474736009697657,
-0.609283436840228));
#36402=CARTESIAN_POINT('Ctrl Pts',(-0.193724355669966,-0.0320616771995824,
-0.610193301489344));
#36403=CARTESIAN_POINT('Ctrl Pts',(-0.195517139945011,-0.0161345209525238,
-0.611103166138461));
#36404=CARTESIAN_POINT('Ctrl Pts',(-0.195373814288334,-0.000175590164213202,
-0.612013030787577));
#36405=CARTESIAN_POINT('Ctrl Pts',(-0.195382883542994,-0.000175680656981076,
-0.622186969212423));
#36406=CARTESIAN_POINT('Ctrl Pts',(-0.19552412444615,-0.0158270061181529,
-0.621294536349111));
#36407=CARTESIAN_POINT('Ctrl Pts',(-0.193800270478103,-0.0314476057070434,
-0.620402103485799));
#36408=CARTESIAN_POINT('Ctrl Pts',(-0.190091640716924,-0.0465818348493538,
-0.619509670622488));
#36409=CARTESIAN_POINT('Ctrl Pts',(-0.174746412471808,-0.109202860796361,
-0.615817043732547));
#36410=CARTESIAN_POINT('Ctrl Pts',(-0.125420571841566,-0.163496918187019,
-0.612124416842606));
#36411=CARTESIAN_POINT('Ctrl Pts',(-0.0645549580566868,-0.184762953588956,
-0.608431789952666));
#36412=CARTESIAN_POINT('Ctrl Pts',(-0.0036893442718077,-0.206028988990894,
-0.604739163062725));
#36413=CARTESIAN_POINT('Ctrl Pts',(0.0687160426677074,-0.19426700240411,
-0.601046536172783));
#36414=CARTESIAN_POINT('Ctrl Pts',(0.119720342167793,-0.154828085566673,
-0.597353909282843));
#36415=CARTESIAN_POINT('Ctrl Pts',(0.170724641667879,-0.115389168729235,
-0.593661282392902));
#36416=CARTESIAN_POINT('Ctrl Pts',(0.200327853728537,-0.0482733216411438,
-0.589968655502962));
#36417=CARTESIAN_POINT('Ctrl Pts',(0.195061974822576,0.015985047408839,
-0.586276028613022));
#36418=CARTESIAN_POINT('Ctrl Pts',(0.189796095916616,0.0802434164588218,
-0.582583401723081));
#36419=CARTESIAN_POINT('Ctrl Pts',(0.149661126044039,0.141644307470696,
-0.578890774833139));
#36420=CARTESIAN_POINT('Ctrl Pts',(0.092916495169642,0.172253359155183,
-0.575198147943198));
#36421=CARTESIAN_POINT('Ctrl Pts',(0.0361718642952446,0.20286241083967,
-0.571505521053257));
#36422=CARTESIAN_POINT('Ctrl Pts',(-0.0371824275809728,0.202679623196771,
-0.567812894163317));
#36423=CARTESIAN_POINT('Ctrl Pts',(-0.0937738058612257,0.171788151132837,
-0.564120267273376));
#36424=CARTESIAN_POINT('Ctrl Pts',(-0.150365184141479,0.140896679068903,
-0.560427640383436));
#36425=CARTESIAN_POINT('Ctrl Pts',(-0.190193648825767,0.0792965225839352,
-0.556735013493495));
#36426=CARTESIAN_POINT('Ctrl Pts',(-0.195139216797218,0.0150127096795879,
-0.553042386603554));
#36427=CARTESIAN_POINT('Ctrl Pts',(-0.195521106165581,0.010048809709412,
-0.552757247473177));
#36428=CARTESIAN_POINT('Ctrl Pts',(-0.195694999368898,0.00506890790750389,
-0.5524721083428));
#36429=CARTESIAN_POINT('Ctrl Pts',(-0.195667167474188,8.703216064893E-5,
-0.552186969212423));
#36430=CARTESIAN_POINT('Origin',(0.,0.,-0.385));
#36431=CARTESIAN_POINT('',(-0.195144246227183,0.000106621721020397,-0.472013030787577));
#36432=CARTESIAN_POINT('',(-0.195139240617864,0.000102604098994689,-0.482186969212423));
#36433=CARTESIAN_POINT('',(-0.1954,-2.39295984553393E-17,-0.385));
#36434=CARTESIAN_POINT('Ctrl Pts',(-0.195144246227183,0.000106621721020397,
-0.472013030787577));
#36435=CARTESIAN_POINT('Ctrl Pts',(-0.195271140890506,0.0255321757748805,
-0.473458310125838));
#36436=CARTESIAN_POINT('Ctrl Pts',(-0.190654961237712,0.0509134566429959,
-0.474903589464099));
#36437=CARTESIAN_POINT('Ctrl Pts',(-0.181080042024378,0.0742611522024674,
-0.476348868802359));
#36438=CARTESIAN_POINT('Ctrl Pts',(-0.156616532984865,0.133913515699754,
-0.4800414956923));
#36439=CARTESIAN_POINT('Ctrl Pts',(-0.0997833319551522,0.180291027942414,
-0.483734122582241));
#36440=CARTESIAN_POINT('Ctrl Pts',(-0.0364367355576039,0.19229421376834,
-0.487426749472182));
#36441=CARTESIAN_POINT('Ctrl Pts',(0.0269098608399439,0.204297399594266,
-0.491119376362123));
#36442=CARTESIAN_POINT('Ctrl Pts',(0.0967698526053274,0.181926259003459,
-0.494812003252064));
#36443=CARTESIAN_POINT('Ctrl Pts',(0.141360397382926,0.135358554943971,
-0.498504630142004));
#36444=CARTESIAN_POINT('Ctrl Pts',(0.185950942160524,0.0887908508844819,
-0.502197257031945));
#36445=CARTESIAN_POINT('Ctrl Pts',(0.205272039950337,0.0180265833563106,
-0.505889883921886));
#36446=CARTESIAN_POINT('Ctrl Pts',(0.190533546493163,-0.0447400045445576,
-0.509582510811826));
#36447=CARTESIAN_POINT('Ctrl Pts',(0.175795053035988,-0.107506592445426,
-0.513275137701767));
#36448=CARTESIAN_POINT('Ctrl Pts',(0.126996968331827,-0.162275500718991,
-0.516967764591708));
#36449=CARTESIAN_POINT('Ctrl Pts',(0.0663400083406457,-0.184129583838522,
-0.520660391481649));
#36450=CARTESIAN_POINT('Ctrl Pts',(0.00568304834946542,-0.205983666958053,
-0.52435301837159));
#36451=CARTESIAN_POINT('Ctrl Pts',(-0.0668327869287337,-0.19492292492355,
-0.528045645261531));
#36452=CARTESIAN_POINT('Ctrl Pts',(-0.118216377660041,-0.155979448611229,
-0.531738272151471));
#36453=CARTESIAN_POINT('Ctrl Pts',(-0.165874770845197,-0.119859288854497,
-0.53516319169684));
#36454=CARTESIAN_POINT('Ctrl Pts',(-0.195353932541471,-0.0597527191423684,
-0.538588111242208));
#36455=CARTESIAN_POINT('Ctrl Pts',(-0.195672562949621,8.22112365601695E-5,
-0.542013030787577));
#36456=CARTESIAN_POINT('Ctrl Pts',(-0.195667167474188,8.703216064893E-5,
-0.552186969212423));
#36457=CARTESIAN_POINT('Ctrl Pts',(-0.19533456899701,-0.059447696042551,
-0.548779481452859));
#36458=CARTESIAN_POINT('Ctrl Pts',(-0.166193851506661,-0.119264320953253,
-0.545371993693295));
#36459=CARTESIAN_POINT('Ctrl Pts',(-0.118947235469162,-0.155422811859585,
-0.541964505933731));
#36460=CARTESIAN_POINT('Ctrl Pts',(-0.0677470149110404,-0.194607051170686,
-0.538271879043791));
#36461=CARTESIAN_POINT('Ctrl Pts',(0.00471609746381744,-0.20600806046916,
-0.53457925215385));
#36462=CARTESIAN_POINT('Ctrl Pts',(0.0654749683434781,-0.184438943551293,
-0.530886625263909));
#36463=CARTESIAN_POINT('Ctrl Pts',(0.126233839223138,-0.162869826633425,
-0.527193998373969));
#36464=CARTESIAN_POINT('Ctrl Pts',(0.175288468607602,-0.108330583499217,
-0.523501371484028));
#36465=CARTESIAN_POINT('Ctrl Pts',(0.190321425282009,-0.0456338736779784,
-0.519808744594087));
#36466=CARTESIAN_POINT('Ctrl Pts',(0.205354381956416,0.0170628361432606,
-0.516116117704146));
#36467=CARTESIAN_POINT('Ctrl Pts',(0.186365665920766,0.0879170126515298,
-0.512423490814205));
#36468=CARTESIAN_POINT('Ctrl Pts',(0.141994204226371,0.134693508760327,
-0.508730863924265));
#36469=CARTESIAN_POINT('Ctrl Pts',(0.0976227425319756,0.181470004869124,
-0.505038237034324));
#36470=CARTESIAN_POINT('Ctrl Pts',(0.0278685351788353,0.204168820578448,
-0.501345610144383));
#36471=CARTESIAN_POINT('Ctrl Pts',(-0.0355337021850324,0.19246311688275,
-0.497652983254443));
#36472=CARTESIAN_POINT('Ctrl Pts',(-0.0989359395488994,0.180757413187051,
-0.493960356364502));
#36473=CARTESIAN_POINT('Ctrl Pts',(-0.155986206923494,0.134647190086329,
-0.49026772947456));
#36474=CARTESIAN_POINT('Ctrl Pts',(-0.180729453215574,0.0751103194393806,
-0.48657510258462));
#36475=CARTESIAN_POINT('Ctrl Pts',(-0.19053066592285,0.0515267715795701,
-0.485112391460554));
#36476=CARTESIAN_POINT('Ctrl Pts',(-0.195262634724071,0.0258364695538892,
-0.483649680336489));
#36477=CARTESIAN_POINT('Ctrl Pts',(-0.195139240617864,0.000102604098994689,
-0.482186969212423));
#36478=CARTESIAN_POINT('Origin',(0.,0.,-0.385));
#36479=CARTESIAN_POINT('',(-0.195293314183532,-0.000167834691889468,-0.402013030787577));
#36480=CARTESIAN_POINT('',(-0.195301750645145,-0.000169271322796084,-0.412186969212423));
#36481=CARTESIAN_POINT('',(-0.1954,-2.39295984553393E-17,-0.385));
#36482=CARTESIAN_POINT('Ctrl Pts',(-0.195293314183532,-0.000167834691889468,
-0.402013030787577));
#36483=CARTESIAN_POINT('Ctrl Pts',(-0.194911528013015,0.0458849723600842,
-0.404635882119527));
#36484=CARTESIAN_POINT('Ctrl Pts',(-0.178618575845566,0.0921809008404429,
-0.407258733451476));
#36485=CARTESIAN_POINT('Ctrl Pts',(-0.148897030686981,0.127021158074873,
-0.409881584783426));
#36486=CARTESIAN_POINT('Ctrl Pts',(-0.107053036127976,0.176071620504506,
-0.413574211673367));
#36487=CARTESIAN_POINT('Ctrl Pts',(-0.0385923533484633,0.202415904400708,
-0.417266838563308));
#36488=CARTESIAN_POINT('Ctrl Pts',(0.0253387916998359,0.194068663058447,
-0.420959465453248));
#36489=CARTESIAN_POINT('Ctrl Pts',(0.0892699367481351,0.185721421716186,
-0.424652092343189));
#36490=CARTESIAN_POINT('Ctrl Pts',(0.148671544065221,0.142682655135463,
-0.42834471923313));
#36491=CARTESIAN_POINT('Ctrl Pts',(0.176518819151958,0.0845328742635806,
-0.43203734612307));
#36492=CARTESIAN_POINT('Ctrl Pts',(0.204366094238696,0.0263830933916977,
-0.435729973013011));
#36493=CARTESIAN_POINT('Ctrl Pts',(0.200659037095084,-0.0468777017713445,
-0.439422599902952));
#36494=CARTESIAN_POINT('Ctrl Pts',(0.167084175443548,-0.101919471458649,
-0.443115226792893));
#36495=CARTESIAN_POINT('Ctrl Pts',(0.133509313792012,-0.156961241145953,
-0.446807853682834));
#36496=CARTESIAN_POINT('Ctrl Pts',(0.0700666476325517,-0.193783985357519,
-0.450500480572774));
#36497=CARTESIAN_POINT('Ctrl Pts',(0.00561945344688623,-0.195635176001563,
-0.454193107462715));
#36498=CARTESIAN_POINT('Ctrl Pts',(-0.0588277407387793,-0.197486366645606,
-0.457885734352656));
#36499=CARTESIAN_POINT('Ctrl Pts',(-0.12427946295065,-0.164366003722127,
-0.461578361242597));
#36500=CARTESIAN_POINT('Ctrl Pts',(-0.160958415531928,-0.11134221488443,
-0.465270988132538));
#36501=CARTESIAN_POINT('Ctrl Pts',(-0.1832813733445,-0.0790717240991829,
-0.467518335684218));
#36502=CARTESIAN_POINT('Ctrl Pts',(-0.194946930453413,-0.0394290272987776,
-0.469765683235897));
#36503=CARTESIAN_POINT('Ctrl Pts',(-0.195144246227183,0.000106621721020397,
-0.472013030787577));
#36504=CARTESIAN_POINT('Ctrl Pts',(-0.195139240617864,0.000102604098994689,
-0.482186969212423));
#36505=CARTESIAN_POINT('Ctrl Pts',(-0.194951125235189,-0.0391288964691331,
-0.479957053446548));
#36506=CARTESIAN_POINT('Ctrl Pts',(-0.1834785316021,-0.0784616439633596,
-0.477727137680673));
#36507=CARTESIAN_POINT('Ctrl Pts',(-0.161479272427984,-0.110585441722134,
-0.475497221914798));
#36508=CARTESIAN_POINT('Ctrl Pts',(-0.125049620138749,-0.163780814043522,
-0.471804595024857));
#36509=CARTESIAN_POINT('Ctrl Pts',(-0.0597540903507157,-0.197208040493121,
-0.468111968134916));
#36510=CARTESIAN_POINT('Ctrl Pts',(0.00470107911431957,-0.195659385673228,
-0.464419341244975));
#36511=CARTESIAN_POINT('Ctrl Pts',(0.0691562485793548,-0.194110730853336,
-0.460726714355034));
#36512=CARTESIAN_POINT('Ctrl Pts',(0.132771057721392,-0.157586194763953,
-0.457034087465094));
#36513=CARTESIAN_POINT('Ctrl Pts',(0.166603913510149,-0.10270263555075,
-0.453341460575153));
#36514=CARTESIAN_POINT('Ctrl Pts',(0.200436769298907,-0.0478190763375483,
-0.449648833685212));
#36515=CARTESIAN_POINT('Ctrl Pts',(0.204487671734386,0.0254235059994729,
-0.445956206795272));
#36516=CARTESIAN_POINT('Ctrl Pts',(0.176913660487352,0.0837033576319605,
-0.442263579905331));
#36517=CARTESIAN_POINT('Ctrl Pts',(0.149339649240319,0.141983209264448,
-0.43857095301539));
#36518=CARTESIAN_POINT('Ctrl Pts',(0.0901407243107727,0.185300330192403,
-0.434878326125449));
#36519=CARTESIAN_POINT('Ctrl Pts',(0.0262494697315635,0.193947572000777,
-0.431185699235508));
#36520=CARTESIAN_POINT('Ctrl Pts',(-0.0376417848476453,0.202594813809151,
-0.427493072345568));
#36521=CARTESIAN_POINT('Ctrl Pts',(-0.106225369076517,0.176572176497946,
-0.423800445455627));
#36522=CARTESIAN_POINT('Ctrl Pts',(-0.148299142919833,0.127718673479187,
-0.420107818565686));
#36523=CARTESIAN_POINT('Ctrl Pts',(-0.178382516650695,0.092787692606204,
-0.417467535447932));
#36524=CARTESIAN_POINT('Ctrl Pts',(-0.194912849038005,0.0461845170874172,
-0.414827252330178));
#36525=CARTESIAN_POINT('Ctrl Pts',(-0.195301750645145,-0.000169271322796084,
-0.412186969212423));
#36526=CARTESIAN_POINT('Origin',(0.,0.,-0.385));
#36527=CARTESIAN_POINT('',(-0.195708263869822,3.44180068116273E-5,-0.332013030787577));
#36528=CARTESIAN_POINT('',(-0.195705679436412,3.98752641654602E-5,-0.342186969212424));
#36529=CARTESIAN_POINT('',(-0.1954,-2.39295984553393E-17,-0.385));
#36530=CARTESIAN_POINT('Ctrl Pts',(-0.195708263869822,3.44180068116273E-5,
-0.332013030787577));
#36531=CARTESIAN_POINT('Ctrl Pts',(-0.195712867835684,0.0019167555331574,
-0.332120827223275));
#36532=CARTESIAN_POINT('Ctrl Pts',(-0.195688044184301,0.00379896863771164,
-0.332228623658972));
#36533=CARTESIAN_POINT('Ctrl Pts',(-0.195633418288648,0.00568031641885265,
-0.33233642009467));
#36534=CARTESIAN_POINT('Ctrl Pts',(-0.193762177835561,0.0701269315691545,
-0.336029046984611));
#36535=CARTESIAN_POINT('Ctrl Pts',(-0.156919698023893,0.133558138888658,
-0.339721673874551));
#36536=CARTESIAN_POINT('Ctrl Pts',(-0.101867485665295,0.167115875099989,
-0.343414300764492));
#36537=CARTESIAN_POINT('Ctrl Pts',(-0.0468152733066967,0.200673611311319,
-0.347106927654433));
#36538=CARTESIAN_POINT('Ctrl Pts',(0.026446671598832,0.204357876414479,
-0.350799554544373));
#36539=CARTESIAN_POINT('Ctrl Pts',(0.084587786207124,0.176492511939285,
-0.354492181434314));
#36540=CARTESIAN_POINT('Ctrl Pts',(0.142728900815417,0.14862714746409,-0.358184808324255));
#36541=CARTESIAN_POINT('Ctrl Pts',(0.185749185126472,0.089212153410541,
-0.361877435214196));
#36542=CARTESIAN_POINT('Ctrl Pts',(0.194076536712586,0.0252784145806732,
-0.365570062104137));
#36543=CARTESIAN_POINT('Ctrl Pts',(0.202403888298699,-0.0386553242491941,
-0.369262688994078));
#36544=CARTESIAN_POINT('Ctrl Pts',(0.17603830715987,-0.10710780785538,-0.372955315884018));
#36545=CARTESIAN_POINT('Ctrl Pts',(0.126974829193245,-0.148936540504495,
-0.376647942773959));
#36546=CARTESIAN_POINT('Ctrl Pts',(0.07791135122662,-0.19076527315361,-0.3803405696639));
#36547=CARTESIAN_POINT('Ctrl Pts',(0.00614997643219979,-0.205970254845654,
-0.384033196553841));
#36548=CARTESIAN_POINT('Ctrl Pts',(-0.0556614175584705,-0.187633970648876,
-0.387725823443782));
#36549=CARTESIAN_POINT('Ctrl Pts',(-0.117472811549142,-0.169297686452097,
-0.391418450333722));
#36550=CARTESIAN_POINT('Ctrl Pts',(-0.169334224736063,-0.117420136366495,
-0.395111077223663));
#36551=CARTESIAN_POINT('Ctrl Pts',(-0.187651278160274,-0.0556030408421606,
-0.398803704113603));
#36552=CARTESIAN_POINT('Ctrl Pts',(-0.192957835424703,-0.0376942675409406,
-0.399873479671594));
#36553=CARTESIAN_POINT('Ctrl Pts',(-0.195449032316932,-0.0189512734483915,
-0.400943255229586));
#36554=CARTESIAN_POINT('Ctrl Pts',(-0.195293314183532,-0.000167834691889468,
-0.402013030787577));
#36555=CARTESIAN_POINT('Ctrl Pts',(-0.195301750645145,-0.000169271322796084,
-0.412186969212423));
#36556=CARTESIAN_POINT('Ctrl Pts',(-0.195456756061615,-0.0186446083890101,
-0.411134625440237));
#36557=CARTESIAN_POINT('Ctrl Pts',(-0.193047535469114,-0.0370803278451861,
-0.41008228166805));
#36558=CARTESIAN_POINT('Ctrl Pts',(-0.187910199406209,-0.0547215890226383,
-0.409029937895864));
#36559=CARTESIAN_POINT('Ctrl Pts',(-0.169883518591507,-0.11662397977939,
-0.405337311005923));
#36560=CARTESIAN_POINT('Ctrl Pts',(-0.11826619350434,-0.168744392566579,
-0.401644684115982));
#36561=CARTESIAN_POINT('Ctrl Pts',(-0.0565415550860151,-0.187370616411795,
-0.397952057226041));
#36562=CARTESIAN_POINT('Ctrl Pts',(0.0051830833323095,-0.20599684025701,
-0.394259430336101));
#36563=CARTESIAN_POINT('Ctrl Pts',(0.0770150350817921,-0.191128875160252,
-0.39056680344616));
#36564=CARTESIAN_POINT('Ctrl Pts',(0.126274313505723,-0.149530910164822,
-0.386874176556219));
#36565=CARTESIAN_POINT('Ctrl Pts',(0.175533591929654,-0.107932945169391,
-0.383181549666278));
#36566=CARTESIAN_POINT('Ctrl Pts',(0.202220197028032,-0.0396049802752874,
-0.379488922776338));
#36567=CARTESIAN_POINT('Ctrl Pts',(0.194193042873466,0.0243671386421074,
-0.375796295886397));
#36568=CARTESIAN_POINT('Ctrl Pts',(0.1861658887189,0.0883392575595017,-0.372103668996456));
#36569=CARTESIAN_POINT('Ctrl Pts',(0.143424975311391,0.147955530500188,
-0.368411042106515));
#36570=CARTESIAN_POINT('Ctrl Pts',(0.0854153051300223,0.176093500719381,
-0.364718415216575));
#36571=CARTESIAN_POINT('Ctrl Pts',(0.0274056349486537,0.204231470938575,
-0.361025788326634));
#36572=CARTESIAN_POINT('Ctrl Pts',(-0.0458727920065736,0.200891138436277,
-0.357333161436693));
#36573=CARTESIAN_POINT('Ctrl Pts',(-0.101081914374396,0.167592189354063,
-0.353640534546752));
#36574=CARTESIAN_POINT('Ctrl Pts',(-0.156291036742218,0.134293240271849,
-0.349947907656811));
#36575=CARTESIAN_POINT('Ctrl Pts',(-0.193430854522634,0.0710356746097188,
-0.346255280766871));
#36576=CARTESIAN_POINT('Ctrl Pts',(-0.195604586827451,0.00659855727457022,
-0.34256265387693));
#36577=CARTESIAN_POINT('Ctrl Pts',(-0.195678304708696,0.00441329842142617,
-0.342437425655428));
#36578=CARTESIAN_POINT('Ctrl Pts',(-0.195711808283359,0.00222668297225595,
-0.342312197433926));
#36579=CARTESIAN_POINT('Ctrl Pts',(-0.195705679436412,3.98752641654602E-5,
-0.342186969212424));
#36580=CARTESIAN_POINT('Origin',(0.,0.,-0.385));
#36581=CARTESIAN_POINT('',(-0.19519881356068,0.000139152780809226,-0.262013030787577));
#36582=CARTESIAN_POINT('',(-0.195192130579109,0.000136023405943259,-0.272186969212423));
#36583=CARTESIAN_POINT('',(-0.1954,-2.39295984553393E-17,-0.385));
#36584=CARTESIAN_POINT('Ctrl Pts',(-0.19519881356068,0.000139152780809226,
-0.262013030787577));
#36585=CARTESIAN_POINT('Ctrl Pts',(-0.195348727543358,0.0227356530869617,
-0.263298399216963));
#36586=CARTESIAN_POINT('Ctrl Pts',(-0.191722703742678,0.0452855435778098,
-0.26458376764635));
#36587=CARTESIAN_POINT('Ctrl Pts',(-0.184108936130051,0.0663972888993632,
-0.265869136075736));
#36588=CARTESIAN_POINT('Ctrl Pts',(-0.162235983303931,0.127047447006306,
-0.269561762965677));
#36589=CARTESIAN_POINT('Ctrl Pts',(-0.107451896378664,0.175828490457768,
-0.273254389855617));
#36590=CARTESIAN_POINT('Ctrl Pts',(-0.0446807262998327,0.190547456158574,
-0.276947016745558));
#36591=CARTESIAN_POINT('Ctrl Pts',(0.0180904437789986,0.20526642185938,
-0.280639643635499));
#36592=CARTESIAN_POINT('Ctrl Pts',(0.0888486970113934,0.18592330980953,
-0.28433227052544));
#36593=CARTESIAN_POINT('Ctrl Pts',(0.135402526447063,0.141318279701041,
-0.288024897415381));
#36594=CARTESIAN_POINT('Ctrl Pts',(0.181956355882732,0.0967132495925533,
-0.291717524305321));
#36595=CARTESIAN_POINT('Ctrl Pts',(0.204305761521676,0.0268463014254276,
-0.295410151195262));
#36596=CARTESIAN_POINT('Ctrl Pts',(0.192282868776658,-0.0364965576431119,
-0.299102778085202));
#36597=CARTESIAN_POINT('Ctrl Pts',(0.18025997603164,-0.0998394167116532,
-0.302795404975143));
#36598=CARTESIAN_POINT('Ctrl Pts',(0.133864784902659,-0.156658186681608,
-0.306488031865084));
#36599=CARTESIAN_POINT('Ctrl Pts',(0.0742048135540952,-0.181103136340265,
-0.310180658755025));
#36600=CARTESIAN_POINT('Ctrl Pts',(0.0145448422055335,-0.205548085998922,
-0.313873285644966));
#36601=CARTESIAN_POINT('Ctrl Pts',(-0.058379909362609,-0.197619215346285,
-0.317565912534907));
#36602=CARTESIAN_POINT('Ctrl Pts',(-0.111392284599426,-0.160923768529416,
-0.321258539424847));
#36603=CARTESIAN_POINT('Ctrl Pts',(-0.162857104323945,-0.125299547831808,
-0.32484336987909));
#36604=CARTESIAN_POINT('Ctrl Pts',(-0.195555156423111,-0.0625637638898928,
-0.328428200333334));
#36605=CARTESIAN_POINT('Ctrl Pts',(-0.195708263869822,3.44180068116273E-5,
-0.332013030787577));
#36606=CARTESIAN_POINT('Ctrl Pts',(-0.195705679436412,3.98752641654602E-5,
-0.342186969212424));
#36607=CARTESIAN_POINT('Ctrl Pts',(-0.195531085880929,-0.0622561057247903,
-0.338619570543985));
#36608=CARTESIAN_POINT('Ctrl Pts',(-0.16319401629578,-0.124708108542943,
-0.335052171875546));
#36609=CARTESIAN_POINT('Ctrl Pts',(-0.112146426745488,-0.160399109455942,
-0.331484773207107));
#36610=CARTESIAN_POINT('Ctrl Pts',(-0.0593068875294896,-0.197342989843137,
-0.327792146317167));
#36611=CARTESIAN_POINT('Ctrl Pts',(0.0135798377317254,-0.205614081609361,
-0.324099519427226));
#36612=CARTESIAN_POINT('Ctrl Pts',(0.0733538925813345,-0.181449446924897,
-0.320406892537285));
#36613=CARTESIAN_POINT('Ctrl Pts',(0.133127947430945,-0.157284812240432,
-0.316714265647345));
#36614=CARTESIAN_POINT('Ctrl Pts',(0.179789331868949,-0.100684451105276,
-0.313021638757404));
#36615=CARTESIAN_POINT('Ctrl Pts',(0.19210942292752,-0.0373987295018618,
-0.309329011867463));
#36616=CARTESIAN_POINT('Ctrl Pts',(0.204429513986091,0.025886992101553,
-0.305636384977522));
#36617=CARTESIAN_POINT('Ctrl Pts',(0.18240831166523,0.0958580741732274,
-0.301943758087581));
#36618=CARTESIAN_POINT('Ctrl Pts',(0.136064374285097,0.140681133761328,
-0.298251131197641));
#36619=CARTESIAN_POINT('Ctrl Pts',(0.0897204369049655,0.185504193349427,
-0.2945585043077));
#36620=CARTESIAN_POINT('Ctrl Pts',(0.0190537644655635,0.205179230453953,
-0.290865877417759));
#36621=CARTESIAN_POINT('Ctrl Pts',(-0.0437858008467183,0.190755075924799,
-0.287173250527818));
#36622=CARTESIAN_POINT('Ctrl Pts',(-0.106625366159001,0.176330921395644,
-0.283480623637877));
#36623=CARTESIAN_POINT('Ctrl Pts',(-0.161637824344163,0.127807575232807,
-0.279787996747937));
#36624=CARTESIAN_POINT('Ctrl Pts',(-0.183795226765297,0.0672607609460622,
-0.276095369857996));
#36625=CARTESIAN_POINT('Ctrl Pts',(-0.191612607048412,0.045899165249305,
-0.274792569642805));
#36626=CARTESIAN_POINT('Ctrl Pts',(-0.195340329287759,0.0230409392171715,
-0.273489769427614));
#36627=CARTESIAN_POINT('Ctrl Pts',(-0.195192130579109,0.000136023405943259,
-0.272186969212423));
#36628=CARTESIAN_POINT('Origin',(0.,0.,-0.385));
#36629=CARTESIAN_POINT('',(-0.195221192409109,-0.000148384978497854,-0.192013030787577));
#36630=CARTESIAN_POINT('',(-0.195228501957461,-0.000151029643043509,-0.202186969212423));
#36631=CARTESIAN_POINT('',(-0.1954,-2.39295984553393E-17,-0.385));
#36632=CARTESIAN_POINT('Ctrl Pts',(-0.195221192409109,-0.000148384978497854,
-0.192013030787577));
#36633=CARTESIAN_POINT('Ctrl Pts',(-0.194912521452068,0.0431370728685057,
-0.194475971210652));
#36634=CARTESIAN_POINT('Ctrl Pts',(-0.18070219546031,0.0866065747243266,
-0.196938911633727));
#36635=CARTESIAN_POINT('Ctrl Pts',(-0.154226937755701,0.120493781946361,
-0.199401852056802));
#36636=CARTESIAN_POINT('Ctrl Pts',(-0.114533225474957,0.171300050518968,
-0.203094478946743));
#36637=CARTESIAN_POINT('Ctrl Pts',(-0.0472700584410176,0.200566970604116,
-0.206787105836683));
#36638=CARTESIAN_POINT('Ctrl Pts',(0.016961151042017,0.194979537104919,
-0.210479732726624));
#36639=CARTESIAN_POINT('Ctrl Pts',(0.0811923605250517,0.189392103605722,
-0.214172359616565));
#36640=CARTESIAN_POINT('Ctrl Pts',(0.142391612457181,0.148950316522181,
-0.217864986506506));
#36641=CARTESIAN_POINT('Ctrl Pts',(0.172716271241626,0.0920531913214624,
-0.221557613396447));
#36642=CARTESIAN_POINT('Ctrl Pts',(0.20304093002607,0.0351560661207439,
-0.225250240286387));
#36643=CARTESIAN_POINT('Ctrl Pts',(0.202490995662829,-0.0381963971971516,
-0.228942867176328));
#36644=CARTESIAN_POINT('Ctrl Pts',(0.17131666197679,-0.0946324553291228,
-0.232635494066269));
#36645=CARTESIAN_POINT('Ctrl Pts',(0.140142328290751,-0.151068513461093,
-0.236328120956209));
#36646=CARTESIAN_POINT('Ctrl Pts',(0.0783435952819142,-0.19058816640714,
-0.24002074784615));
#36647=CARTESIAN_POINT('Ctrl Pts',(0.0140358306636315,-0.195211925443371,
-0.243713374736091));
#36648=CARTESIAN_POINT('Ctrl Pts',(-0.0502719339546524,-0.199835684479602,
-0.247406001626032));
#36649=CARTESIAN_POINT('Ctrl Pts',(-0.117088730182383,-0.169563549606015,
-0.251098628515973));
#36650=CARTESIAN_POINT('Ctrl Pts',(-0.156016218932762,-0.11816784578801,
-0.254791255405913));
#36651=CARTESIAN_POINT('Ctrl Pts',(-0.181393417722536,-0.0846624994479597,
-0.257198513866468));
#36652=CARTESIAN_POINT('Ctrl Pts',(-0.194918052266947,-0.042179932780427,
-0.259605772327022));
#36653=CARTESIAN_POINT('Ctrl Pts',(-0.19519881356068,0.000139152780809226,
-0.262013030787577));
#36654=CARTESIAN_POINT('Ctrl Pts',(-0.195192130579109,0.000136023405943259,
-0.272186969212423));
#36655=CARTESIAN_POINT('Ctrl Pts',(-0.19492027828513,-0.0418802260161198,
-0.269797142537674));
#36656=CARTESIAN_POINT('Ctrl Pts',(-0.181606189342149,-0.0840535836858002,
-0.267407315862924));
#36657=CARTESIAN_POINT('Ctrl Pts',(-0.156569170098022,-0.117434195704244,
-0.265017489188174));
#36658=CARTESIAN_POINT('Ctrl Pts',(-0.117883364352505,-0.169012055657157,
-0.261324862298233));
#36659=CARTESIAN_POINT('Ctrl Pts',(-0.051209406204363,-0.19959749315233,
-0.257632235408292));
#36660=CARTESIAN_POINT('Ctrl Pts',(0.0131193497373221,-0.195275646237997,
-0.253939608518351));
#36661=CARTESIAN_POINT('Ctrl Pts',(0.0774481056790059,-0.190953799323664,
-0.25024698162841));
#36662=CARTESIAN_POINT('Ctrl Pts',(0.139431659414233,-0.151724667999826,
-0.24655435473847));
#36663=CARTESIAN_POINT('Ctrl Pts',(0.170870558530041,-0.0954355676028622,
-0.242861727848529));
#36664=CARTESIAN_POINT('Ctrl Pts',(0.202309457645848,-0.0391464672058984,
-0.239169100958588));
#36665=CARTESIAN_POINT('Ctrl Pts',(0.203203702142237,0.0342026022641913,
-0.235476474068647));
#36666=CARTESIAN_POINT('Ctrl Pts',(0.17314645488136,0.091241440750627,-0.231783847178707));
#36667=CARTESIAN_POINT('Ctrl Pts',(0.143089207620483,0.148280279237063,
-0.228091220288766));
#36668=CARTESIAN_POINT('Ctrl Pts',(0.0820804686023399,0.189008886739845,
-0.224398593398825));
#36669=CARTESIAN_POINT('Ctrl Pts',(0.0178761979905637,0.194897760180302,
-0.220705966508884));
#36670=CARTESIAN_POINT('Ctrl Pts',(-0.0463280726212126,0.200786633620759,
-0.217013339618944));
#36671=CARTESIAN_POINT('Ctrl Pts',(-0.113727874826622,0.171835772998892,
-0.213320712729003));
#36672=CARTESIAN_POINT('Ctrl Pts',(-0.153659631261092,0.121216389126229,
-0.209628085839062));
#36673=CARTESIAN_POINT('Ctrl Pts',(-0.180482167591968,0.0872148729344941,
-0.207147713630182));
#36674=CARTESIAN_POINT('Ctrl Pts',(-0.194911299555516,0.0434366593785047,
-0.204667341421303));
#36675=CARTESIAN_POINT('Ctrl Pts',(-0.195228501957461,-0.000151029643043509,
-0.202186969212423));
#36676=CARTESIAN_POINT('Origin',(0.,0.,-0.385));
#36677=CARTESIAN_POINT('',(-0.195714129816575,-1.66459635889404E-5,-0.122013030787577));
#36678=CARTESIAN_POINT('',(-0.195715049123435,-1.11371353569391E-5,-0.132186969212423));
#36679=CARTESIAN_POINT('',(-0.1954,-2.39295984553393E-17,-0.385));
#36680=CARTESIAN_POINT('Ctrl Pts',(-0.195714129816575,-1.66459635889404E-5,
-0.122013030787577));
#36681=CARTESIAN_POINT('Ctrl Pts',(-0.19563573648805,0.0635488758200351,
-0.125653543204341));
#36682=CARTESIAN_POINT('Ctrl Pts',(-0.161767712733412,0.127185954073863,
-0.129294055621104));
#36683=CARTESIAN_POINT('Ctrl Pts',(-0.10896691742764,0.162575785310205,
-0.132934568037868));
#36684=CARTESIAN_POINT('Ctrl Pts',(-0.0554102709350894,0.198472227209985,
-0.136627194927809));
#36685=CARTESIAN_POINT('Ctrl Pts',(0.0176250777221782,0.205306906538936,
-0.140319821817749));
#36686=CARTESIAN_POINT('Ctrl Pts',(0.0769118082973,0.179970218457928,-0.14401244870769));
#36687=CARTESIAN_POINT('Ctrl Pts',(0.136198538872421,0.15463353037692,-0.147705075597631));
#36688=CARTESIAN_POINT('Ctrl Pts',(0.181736651365396,0.0971254748859523,
-0.151397702487572));
#36689=CARTESIAN_POINT('Ctrl Pts',(0.192808475960345,0.0336094599183851,
-0.155090329377513));
#36690=CARTESIAN_POINT('Ctrl Pts',(0.203880300555293,-0.0299065550491812,
-0.158782956267453));
#36691=CARTESIAN_POINT('Ctrl Pts',(0.180485837252216,-0.0994305294933474,
-0.162475583157394));
#36692=CARTESIAN_POINT('Ctrl Pts',(0.133268452240781,-0.1433325374099,-0.166168210047335));
#36693=CARTESIAN_POINT('Ctrl Pts',(0.0860510672293448,-0.187234545326454,
-0.169860836937276));
#36694=CARTESIAN_POINT('Ctrl Pts',(0.0150107605095506,-0.205514586715394,
-0.173553463827216));
#36695=CARTESIAN_POINT('Ctrl Pts',(-0.0475326626638961,-0.189856122850204,
-0.177246090717157));
#36696=CARTESIAN_POINT('Ctrl Pts',(-0.110076085837342,-0.174197658985015,
-0.180938717607098));
#36697=CARTESIAN_POINT('Ctrl Pts',(-0.164122625464441,-0.124600689865696,
-0.184631344497039));
#36698=CARTESIAN_POINT('Ctrl Pts',(-0.185083766514216,-0.0636293967760041,
-0.188323971386979));
#36699=CARTESIAN_POINT('Ctrl Pts',(-0.192064063264259,-0.0433252674354672,
-0.189553657853845));
#36700=CARTESIAN_POINT('Ctrl Pts',(-0.195375304337693,-0.0217597651109067,
-0.190783344320711));
#36701=CARTESIAN_POINT('Ctrl Pts',(-0.195221192409109,-0.000148384978497854,
-0.192013030787577));
#36702=CARTESIAN_POINT('Ctrl Pts',(-0.195228501957461,-0.000151029643043509,
-0.202186969212423));
#36703=CARTESIAN_POINT('Ctrl Pts',(-0.195383531148332,-0.0214540340324061,
-0.200974714531362));
#36704=CARTESIAN_POINT('Ctrl Pts',(-0.192167702584793,-0.0427115286208927,
-0.199762459850301));
#36705=CARTESIAN_POINT('Ctrl Pts',(-0.185380390392341,-0.0627599095134647,
-0.19855020516924));
#36706=CARTESIAN_POINT('Ctrl Pts',(-0.164705682425589,-0.123828917157039,
-0.194857578279299));
#36707=CARTESIAN_POINT('Ctrl Pts',(-0.110892555828552,-0.173679025320728,
-0.191164951389358));
#36708=CARTESIAN_POINT('Ctrl Pts',(-0.0484233240331688,-0.189630897337212,
-0.187472324499417));
#36709=CARTESIAN_POINT('Ctrl Pts',(0.0140459077622141,-0.205582769353695,
-0.183779697609477));
#36710=CARTESIAN_POINT('Ctrl Pts',(0.0851712447559427,-0.187636405222974,
-0.180087070719536));
#36711=CARTESIAN_POINT('Ctrl Pts',(0.132594177669105,-0.14395651726514,
-0.176394443829595));
#36712=CARTESIAN_POINT('Ctrl Pts',(0.180017110582266,-0.100276629307306,
-0.172701816939654));
#36713=CARTESIAN_POINT('Ctrl Pts',(0.203737639414863,-0.0308632175223595,
-0.169009190049713));
#36714=CARTESIAN_POINT('Ctrl Pts',(0.192964091346187,0.0327040549976082,
-0.165316563159773));
#36715=CARTESIAN_POINT('Ctrl Pts',(0.182190543277511,0.0962713275175769,
-0.161623936269832));
#36716=CARTESIAN_POINT('Ctrl Pts',(0.136922918307562,0.153992460772567,
-0.157931309379891));
#36717=CARTESIAN_POINT('Ctrl Pts',(0.0777557571850433,0.179607178680573,
-0.15423868248995));
#36718=CARTESIAN_POINT('Ctrl Pts',(0.0185885960625246,0.205221896588578,
-0.15054605560001));
#36719=CARTESIAN_POINT('Ctrl Pts',(-0.0544781012125634,0.198730199149599,
-0.146853428710069));
#36720=CARTESIAN_POINT('Ctrl Pts',(-0.108202617777375,0.163085514791286,
-0.143160801820128));
#36721=CARTESIAN_POINT('Ctrl Pts',(-0.161422531340639,0.127775620131725,
-0.13950285761756));
#36722=CARTESIAN_POINT('Ctrl Pts',(-0.195661897485078,0.0638578007034306,
-0.135844913414992));
#36723=CARTESIAN_POINT('Ctrl Pts',(-0.195715049123435,-1.11371353569391E-5,
-0.132186969212423));
#36724=CARTESIAN_POINT('Origin',(0.,0.,-0.385));
#36725=CARTESIAN_POINT('',(-0.195265563427387,0.000160747932399612,-0.0520130307875765));
#36726=CARTESIAN_POINT('',(-0.195258838497135,0.000160033407109407,-0.0621869692124234));
#36727=CARTESIAN_POINT('',(-0.1954,-2.39295984553393E-17,-0.385));
#36728=CARTESIAN_POINT('Ctrl Pts',(-0.195265563427387,0.000160747932399612,
-0.0520130307875765));
#36729=CARTESIAN_POINT('Ctrl Pts',(-0.195424699897344,0.0199310521824771,
-0.0531384883080881));
#36730=CARTESIAN_POINT('Ctrl Pts',(-0.192664102409213,0.0396584116229354,
-0.0542639458285998));
#36731=CARTESIAN_POINT('Ctrl Pts',(-0.186800565614977,0.0584146868577315,
-0.0553894033491114));
#36732=CARTESIAN_POINT('Ctrl Pts',(-0.167562297406761,0.119954038654549,
-0.0590820302390522));
#36733=CARTESIAN_POINT('Ctrl Pts',(-0.114920994740183,0.171039702517518,
-0.0627746571289931));
#36734=CARTESIAN_POINT('Ctrl Pts',(-0.0528397488128431,0.188445146666394,
-0.066467284018934));
#36735=CARTESIAN_POINT('Ctrl Pts',(0.00924149711449647,0.205850590815268,
-0.0701599109088748));
#36736=CARTESIAN_POINT('Ctrl Pts',(0.0807626863026003,0.189575815250048,
-0.0738525377988157));
#36737=CARTESIAN_POINT('Ctrl Pts',(0.129192507975583,0.147017210543397,
-0.0775451646887565));
#36738=CARTESIAN_POINT('Ctrl Pts',(0.177622329648565,0.104458605836747,
-0.0812377915786972));
#36739=CARTESIAN_POINT('Ctrl Pts',(0.202960783806429,0.0356161719886669,
-0.0849304184686379));
#36740=CARTESIAN_POINT('Ctrl Pts',(0.193676298191635,-0.0281860789989965,
-0.0886230453585787));
#36741=CARTESIAN_POINT('Ctrl Pts',(0.18439181257684,-0.0919883299866607,
-0.0923156722485195));
#36742=CARTESIAN_POINT('Ctrl Pts',(0.140484387189387,-0.150750398113907,
-0.0960082991384602));
#36743=CARTESIAN_POINT('Ctrl Pts',(0.081931739171364,-0.177740603840422,
-0.099700926028401));
#36744=CARTESIAN_POINT('Ctrl Pts',(0.0233790911533422,-0.204730809566937,
-0.103393552918342));
#36745=CARTESIAN_POINT('Ctrl Pts',(-0.0498187794952493,-0.199949152892722,
-0.107086179808282));
#36746=CARTESIAN_POINT('Ctrl Pts',(-0.104361515224881,-0.165569919440996,
-0.110778806698223));
#36747=CARTESIAN_POINT('Ctrl Pts',(-0.158904250954513,-0.131190685989269,
-0.114471433588164));
#36748=CARTESIAN_POINT('Ctrl Pts',(-0.194791851765185,-0.0672138757600308,
-0.118164060478105));
#36749=CARTESIAN_POINT('Ctrl Pts',(-0.195696680006605,-0.00274636841010696,
-0.121856687368046));
#36750=CARTESIAN_POINT('Ctrl Pts',(-0.195709449952912,-0.00183653097385362,
-0.121908801841223));
#36751=CARTESIAN_POINT('Ctrl Pts',(-0.195715252028656,-0.000926595800520846,
-0.1219609163144));
#36752=CARTESIAN_POINT('Ctrl Pts',(-0.195714129816575,-1.66459635889404E-5,
-0.122013030787577));
#36753=CARTESIAN_POINT('Ctrl Pts',(-0.195715049123435,-1.11371353569391E-5,
-0.132186969212423));
#36754=CARTESIAN_POINT('Ctrl Pts',(-0.195715553079087,-0.000616708538638704,
-0.132152286525051));
#36755=CARTESIAN_POINT('Ctrl Pts',(-0.195712983753233,-0.00122227554755018,
-0.132117603837678));
#36756=CARTESIAN_POINT('Ctrl Pts',(-0.195707328185051,-0.00182781373595469,
-0.132082921150306));
#36757=CARTESIAN_POINT('Ctrl Pts',(-0.195105186173382,-0.0662987866272353,
-0.128390294260365));
#36758=CARTESIAN_POINT('Ctrl Pts',(-0.159518566295507,-0.130443061132149,
-0.124697667370424));
#36759=CARTESIAN_POINT('Ctrl Pts',(-0.105137686353204,-0.165078065539304,
-0.121005040480483));
#36760=CARTESIAN_POINT('Ctrl Pts',(-0.0507568064109017,-0.199713069946459,
-0.117312413590543));
#36761=CARTESIAN_POINT('Ctrl Pts',(0.0224183335958285,-0.204838804255855,
-0.113619786700602));
#36762=CARTESIAN_POINT('Ctrl Pts',(0.0810967868923935,-0.178123499671584,
-0.109927159810661));
#36763=CARTESIAN_POINT('Ctrl Pts',(0.139775240188958,-0.151408195087312,
-0.10623453292072));
#36764=CARTESIAN_POINT('Ctrl Pts',(0.183957006775358,-0.0928518516093715,
-0.10254190603078));
#36765=CARTESIAN_POINT('Ctrl Pts',(0.193541330769425,-0.0290943544827345,
-0.0988492791408388));
#36766=CARTESIAN_POINT('Ctrl Pts',(0.203125654763491,0.034663142643903,
-0.095156652250898));
#36767=CARTESIAN_POINT('Ctrl Pts',(0.178112536165224,0.103621793419236,
-0.0914640253609573));
#36768=CARTESIAN_POINT('Ctrl Pts',(0.129882157652608,0.14640814297767,-0.0877713984710165));
#36769=CARTESIAN_POINT('Ctrl Pts',(0.0816517791399922,0.189194492536102,
-0.0840787715810758));
#36770=CARTESIAN_POINT('Ctrl Pts',(0.0102041407130279,0.205808540877635,
-0.0803861446911351));
#36771=CARTESIAN_POINT('Ctrl Pts',(-0.0519564723881836,0.188693009030546,
-0.0766935178011943));
#36772=CARTESIAN_POINT('Ctrl Pts',(-0.114117085489396,0.171577477183457,
-0.0730008909112535));
#36773=CARTESIAN_POINT('Ctrl Pts',(-0.166990673264856,0.120732365147745,
-0.0693082640213127));
#36774=CARTESIAN_POINT('Ctrl Pts',(-0.1865207333334,0.059287224845946,-0.0656156371313719));
#36775=CARTESIAN_POINT('Ctrl Pts',(-0.192565399493649,0.0402695997597707,
-0.0644727478250558));
#36776=CARTESIAN_POINT('Ctrl Pts',(-0.195415961833315,0.0202365574963669,
-0.0633298585187396));
#36777=CARTESIAN_POINT('Ctrl Pts',(-0.195258838497135,0.000160033407109407,
-0.0621869692124234));
#36778=CARTESIAN_POINT('Origin',(0.,0.,-0.90400562256037));
#36779=CARTESIAN_POINT('',(-0.155442980507318,0.000127964897052157,-0.0290056225603697));
#36780=CARTESIAN_POINT('',(-0.155327760552453,-0.000155038459510079,-0.0151943774396293));
#36781=CARTESIAN_POINT('',(-0.15555,-8.39731161192283E-15,-0.90400562256037));
#36782=CARTESIAN_POINT('',(0.133815347598873,-0.0797905857758447,1.38777878078145E-16));
#36783=CARTESIAN_POINT('Ctrl Pts',(-0.155442980507318,0.000127964897052158,
-0.0290056225603697));
#36784=CARTESIAN_POINT('Ctrl Pts',(-0.155154018602902,-0.035771189888286,
-0.0264384531909407));
#36785=CARTESIAN_POINT('Ctrl Pts',(-0.124961417838318,-0.123741558504079,
-0.0201786569315709));
#36786=CARTESIAN_POINT('Ctrl Pts',(0.0168354762982751,-0.18072128944305,
-0.0105101160781143));
#36787=CARTESIAN_POINT('Ctrl Pts',(0.109303704153288,-0.120379820697564,
-0.00340874459408667));
#36788=CARTESIAN_POINT('Ctrl Pts',(0.133815347598873,-0.0797905857758447,
1.25821662116943E-16));
#36789=CARTESIAN_POINT('',(-0.0319621170202007,-0.152230829911641,0.));
#36790=CARTESIAN_POINT('Origin',(0.,0.,1.11022302462516E-16));
#36791=CARTESIAN_POINT('Ctrl Pts',(-0.155327760552453,-0.000155038459510074,
-0.0151943774396293));
#36792=CARTESIAN_POINT('Ctrl Pts',(-0.155432057916671,-0.0193751812911555,
-0.0138222118496936));
#36793=CARTESIAN_POINT('Ctrl Pts',(-0.143247305876585,-0.090139499299076,
-0.00875741936981715));
#36794=CARTESIAN_POINT('Ctrl Pts',(-0.0824189364736414,-0.141637004936936,
-0.00369262688994078));
#36795=CARTESIAN_POINT('Ctrl Pts',(-0.0319621170202007,-0.152230829911641,
0.));
#36796=CARTESIAN_POINT('Origin',(0.,0.,-0.90400562256037));
#36797=CARTESIAN_POINT('',(-0.155800065982437,-1.32511752194797E-5,-0.0990056225603699));
#36798=CARTESIAN_POINT('',(-0.15543762706361,0.000127396092498608,-0.0851943774396296));
#36799=CARTESIAN_POINT('',(-0.15555,-8.39731161192283E-15,-0.90400562256037));
#36800=CARTESIAN_POINT('Ctrl Pts',(-0.155800065982437,-1.32511752195067E-5,
-0.0990056225603699));
#36801=CARTESIAN_POINT('Ctrl Pts',(-0.155800959329875,-0.00073762526495506,
-0.0989535080871929));
#36802=CARTESIAN_POINT('Ctrl Pts',(-0.155469070736801,-0.0527874635943024,
-0.0952087667240751));
#36803=CARTESIAN_POINT('Ctrl Pts',(-0.0979285564476671,-0.155364913187252,
-0.0877713984710165));
#36804=CARTESIAN_POINT('Ctrl Pts',(0.0768809949247246,-0.16678436092022,
-0.0766935178011943));
#36805=CARTESIAN_POINT('Ctrl Pts',(0.181739746496141,-0.0264500769305604,
-0.0656156371313721));
#36806=CARTESIAN_POINT('Ctrl Pts',(0.121227005284432,0.137957915675413,
-0.0545377564615496));
#36807=CARTESIAN_POINT('Ctrl Pts',(-0.0495783321496912,0.176824978201047,
-0.0434598757917274));
#36808=CARTESIAN_POINT('Ctrl Pts',(-0.146161737697263,0.0830957743134539,
-0.034949164491334));
#36809=CARTESIAN_POINT('Ctrl Pts',(-0.155569662584605,0.0158663007522202,
-0.0301310800808815));
#36810=CARTESIAN_POINT('Ctrl Pts',(-0.155442980507318,0.000127964897052158,
-0.0290056225603697));
#36811=CARTESIAN_POINT('Ctrl Pts',(-0.15543762706361,0.000127396092498587,
-0.0851943774396296));
#36812=CARTESIAN_POINT('Ctrl Pts',(-0.155158579995167,-0.0355280025756548,
-0.0826446398560051));
#36813=CARTESIAN_POINT('Ctrl Pts',(-0.125300184105867,-0.123242688352141,
-0.0764022753824399));
#36814=CARTESIAN_POINT('Ctrl Pts',(0.0201819892413759,-0.182531533674816,
-0.0664672840189338));
#36815=CARTESIAN_POINT('Ctrl Pts',(0.164054917332699,-0.0825830908935778,
-0.0553894033491116));
#36816=CARTESIAN_POINT('Ctrl Pts',(0.158618708021993,0.0925610883157775,
-0.0443115226792891));
#36817=CARTESIAN_POINT('Ctrl Pts',(0.00892266599271826,0.183382072237952,
-0.0332336420094669));
#36818=CARTESIAN_POINT('Ctrl Pts',(-0.129457814449668,0.116933784740767,
-0.0235279269295804));
#36819=CARTESIAN_POINT('Ctrl Pts',(-0.155151383882512,0.0323480340184218,
-0.0175148387396345));
#36820=CARTESIAN_POINT('Ctrl Pts',(-0.155327760552453,-0.000155038459510074,
-0.0151943774396293));
#36821=CARTESIAN_POINT('Origin',(0.,0.,-0.90400562256037));
#36822=CARTESIAN_POINT('',(-0.155407658542666,-0.000118123251820218,-0.16900562256037));
#36823=CARTESIAN_POINT('',(-0.155800797805273,-8.86582091297328E-6,-0.15519437743963));
#36824=CARTESIAN_POINT('',(-0.15555,-8.39731161192283E-15,-0.90400562256037));
#36825=CARTESIAN_POINT('Ctrl Pts',(-0.155407658542666,-0.00011812325182025,
-0.16900562256037));
#36826=CARTESIAN_POINT('Ctrl Pts',(-0.155530340786735,-0.0173220648055368,
-0.167775936093504));
#36827=CARTESIAN_POINT('Ctrl Pts',(-0.144978915679302,-0.086041550229714,
-0.162853622736698));
#36828=CARTESIAN_POINT('Ctrl Pts',(-0.044602845000016,-0.178153809629627,
-0.15423868248995));
#36829=CARTESIAN_POINT('Ctrl Pts',(0.125054059456442,-0.134497815186694,
-0.143160801820128));
#36830=CARTESIAN_POINT('Ctrl Pts',(0.180924204289506,0.0315378177425299,
-0.132082921150306));
#36831=CARTESIAN_POINT('Ctrl Pts',(0.0721710814909035,0.168877296221853,
-0.121005040480484));
#36832=CARTESIAN_POINT('Ctrl Pts',(-0.101429795153458,0.152631651545641,
-0.109979274283838));
#36833=CARTESIAN_POINT('Ctrl Pts',(-0.155737660239083,0.0505886777574477,
-0.102646134977134));
#36834=CARTESIAN_POINT('Ctrl Pts',(-0.155800065982437,-1.32511752195067E-5,
-0.0990056225603699));
#36835=CARTESIAN_POINT('Ctrl Pts',(-0.155800797805273,-8.86582091298835E-6,
-0.15519437743963));
#36836=CARTESIAN_POINT('Ctrl Pts',(-0.15580119898389,-0.000490936607914258,
-0.155159694752257));
#36837=CARTESIAN_POINT('Ctrl Pts',(-0.155581389023891,-0.052298168361465,
-0.151432385174944));
#36838=CARTESIAN_POINT('Ctrl Pts',(-0.0986571866185378,-0.154903070922954,
-0.14401244870769));
#36839=CARTESIAN_POINT('Ctrl Pts',(0.0760980799328472,-0.16714423732766,
-0.132934568037868));
#36840=CARTESIAN_POINT('Ctrl Pts',(0.181612007146477,-0.027301260439323,
-0.121856687368045));
#36841=CARTESIAN_POINT('Ctrl Pts',(0.121876225192118,0.137384278886722,
-0.110778806698223));
#36842=CARTESIAN_POINT('Ctrl Pts',(-0.0487534599252984,0.177061585225392,
-0.0997009260284008));
#36843=CARTESIAN_POINT('Ctrl Pts',(-0.145961746301879,0.0835826589870833,
-0.091172782942203));
#36844=CARTESIAN_POINT('Ctrl Pts',(-0.1555627065669,0.0161095011185192,
-0.0863372667459459));
#36845=CARTESIAN_POINT('Ctrl Pts',(-0.15543762706361,0.000127396092498587,
-0.0851943774396296));
#36846=CARTESIAN_POINT('Origin',(0.,0.,-0.90400562256037));
#36847=CARTESIAN_POINT('',(-0.155389843650787,0.000110773874380199,-0.23900562256037));
#36848=CARTESIAN_POINT('',(-0.155413477377088,-0.000120228561807947,-0.22519437743963));
#36849=CARTESIAN_POINT('',(-0.15555,-8.39731161192283E-15,-0.90400562256037));
#36850=CARTESIAN_POINT('Ctrl Pts',(-0.155389843650787,0.000110773874380203,
-0.23900562256037));
#36851=CARTESIAN_POINT('Ctrl Pts',(-0.155166340993467,-0.0335777305219866,
-0.236598364099816));
#36852=CARTESIAN_POINT('Ctrl Pts',(-0.127884734191329,-0.119272665639336,
-0.23049847874932));
#36853=CARTESIAN_POINT('Ctrl Pts',(0.0131706925618085,-0.183179484648865,
-0.220705966508885));
#36854=CARTESIAN_POINT('Ctrl Pts',(0.160757073107222,-0.0887995151131783,
-0.209628085839062));
#36855=CARTESIAN_POINT('Ctrl Pts',(0.162070414307866,0.0863792310858789,
-0.19855020516924));
#36856=CARTESIAN_POINT('Ctrl Pts',(0.0159157013389389,0.182961421170497,
-0.187472324499417));
#36857=CARTESIAN_POINT('Ctrl Pts',(-0.126889473131666,0.12082536940136,
-0.177624130296461));
#36858=CARTESIAN_POINT('Ctrl Pts',(-0.155161938136486,0.0343396708530999,
-0.171468562983445));
#36859=CARTESIAN_POINT('Ctrl Pts',(-0.155407658542666,-0.00011812325182025,
-0.16900562256037));
#36860=CARTESIAN_POINT('Ctrl Pts',(-0.155413477377088,-0.000120228561807949,
-0.22519437743963));
#36861=CARTESIAN_POINT('Ctrl Pts',(-0.155536889816391,-0.0170786847172067,
-0.223982122758568));
#36862=CARTESIAN_POINT('Ctrl Pts',(-0.14517895913199,-0.0855474016034071,
-0.219077241187567));
#36863=CARTESIAN_POINT('Ctrl Pts',(-0.045438614211677,-0.177942460150977,
-0.210479732726624));
#36864=CARTESIAN_POINT('Ctrl Pts',(0.124421357682504,-0.135083346427328,
-0.199401852056802));
#36865=CARTESIAN_POINT('Ctrl Pts',(0.181070205071097,0.0306882431808897,
-0.18832397138698));
#36866=CARTESIAN_POINT('Ctrl Pts',(0.0729630546502829,0.168536589309041,
-0.177246090717157));
#36867=CARTESIAN_POINT('Ctrl Pts',(-0.100986917449906,0.153081797584407,
-0.166202892734707));
#36868=CARTESIAN_POINT('Ctrl Pts',(-0.155758485945775,0.050834600304081,
-0.158852321642198));
#36869=CARTESIAN_POINT('Ctrl Pts',(-0.155800797805273,-8.86582091298835E-6,
-0.15519437743963));
#36870=CARTESIAN_POINT('Origin',(0.,0.,-0.90400562256037));
#36871=CARTESIAN_POINT('',(-0.155795396340587,2.73987766570263E-5,-0.30900562256037));
#36872=CARTESIAN_POINT('',(-0.155384523600718,0.000108282706206955,-0.29519437743963));
#36873=CARTESIAN_POINT('',(-0.15555,-8.39731161192283E-15,-0.90400562256037));
#36874=CARTESIAN_POINT('Ctrl Pts',(-0.155795396340587,2.73987766570313E-5,
-0.30900562256037));
#36875=CARTESIAN_POINT('Ctrl Pts',(-0.155673513723719,-0.0498044701794957,
-0.305420792106127));
#36876=CARTESIAN_POINT('Ctrl Pts',(-0.102831618486219,-0.151189033169581,
-0.298143334761943));
#36877=CARTESIAN_POINT('Ctrl Pts',(0.0696309893116479,-0.169940330640481,
-0.287173250527819));
#36878=CARTESIAN_POINT('Ctrl Pts',(0.180430968535489,-0.0342469887444786,
-0.276095369857996));
#36879=CARTESIAN_POINT('Ctrl Pts',(0.127056607525184,0.132607726517495,
-0.265017489188174));
#36880=CARTESIAN_POINT('Ctrl Pts',(-0.0419267029707069,0.178802523027537,
-0.253939608518351));
#36881=CARTESIAN_POINT('Ctrl Pts',(-0.144330183939881,0.0876200476939117,
-0.245268986309084));
#36882=CARTESIAN_POINT('Ctrl Pts',(-0.155509184080703,0.0180989295684548,
-0.240290990989756));
#36883=CARTESIAN_POINT('Ctrl Pts',(-0.155389843650787,0.000110773874380203,
-0.23900562256037));
#36884=CARTESIAN_POINT('Ctrl Pts',(-0.155384523600718,0.000108282706206955,
-0.29519437743963));
#36885=CARTESIAN_POINT('Ctrl Pts',(-0.155168113036088,-0.0333391461453875,
-0.29280455076488));
#36886=CARTESIAN_POINT('Ctrl Pts',(-0.128192625181579,-0.118785991398888,
-0.286722097200189));
#36887=CARTESIAN_POINT('Ctrl Pts',(0.0123107014066272,-0.183239277698152,
-0.276947016745558));
#36888=CARTESIAN_POINT('Ctrl Pts',(0.160338466762532,-0.0895531255371017,
-0.265869136075736));
#36889=CARTESIAN_POINT('Ctrl Pts',(0.162474081881463,0.0856175155489654,
-0.254791255405913));
#36890=CARTESIAN_POINT('Ctrl Pts',(0.0167743476807649,0.182884683876359,
-0.243713374736091));
#36891=CARTESIAN_POINT('Ctrl Pts',(-0.126574199990401,0.121310855939487,
-0.23384774874733));
#36892=CARTESIAN_POINT('Ctrl Pts',(-0.155160965434293,0.0345781595001282,
-0.227674749648509));
#36893=CARTESIAN_POINT('Ctrl Pts',(-0.155413477377088,-0.000120228561807949,
-0.22519437743963));
#36894=CARTESIAN_POINT('Origin',(0.,0.,-0.90400562256037));
#36895=CARTESIAN_POINT('',(-0.155465071756645,-0.000133606378324517,-0.37900562256037));
#36896=CARTESIAN_POINT('',(-0.155793338978167,3.17430774774384E-5,-0.36519437743963));
#36897=CARTESIAN_POINT('',(-0.15555,-8.39731161192283E-15,-0.90400562256037));
#36898=CARTESIAN_POINT('Ctrl Pts',(-0.155465071756645,-0.000133606378324543,
-0.37900562256037));
#36899=CARTESIAN_POINT('Ctrl Pts',(-0.155589032635101,-0.0150863387149346,
-0.377935847002379));
#36900=CARTESIAN_POINT('Ctrl Pts',(-0.146760532433313,-0.0815092407522182,
-0.373173444554447));
#36901=CARTESIAN_POINT('Ctrl Pts',(-0.0522305681435164,-0.176068618441347,
-0.364718415216575));
#36902=CARTESIAN_POINT('Ctrl Pts',(0.119148375294644,-0.139756414211085,
-0.353640534546752));
#36903=CARTESIAN_POINT('Ctrl Pts',(0.182114078664316,0.023720307768581,
-0.34256265387693));
#36904=CARTESIAN_POINT('Ctrl Pts',(0.0793739779798006,0.165613895153883,
-0.331484773207108));
#36905=CARTESIAN_POINT('Ctrl Pts',(-0.0955885941295399,0.156815213933875,
-0.320406892537285));
#36906=CARTESIAN_POINT('Ctrl Pts',(-0.155102372787945,0.0543511330211424,
-0.312913842321706));
#36907=CARTESIAN_POINT('Ctrl Pts',(-0.15579906137073,0.00152585119335764,
-0.309113418996068));
#36908=CARTESIAN_POINT('Ctrl Pts',(-0.155795396340587,2.73987766570313E-5,
-0.30900562256037));
#36909=CARTESIAN_POINT('Ctrl Pts',(-0.155793338978167,3.1743077477449E-5,
-0.36519437743963));
#36910=CARTESIAN_POINT('Ctrl Pts',(-0.155654352143183,-0.0495595560158264,
-0.361626978771191));
#36911=CARTESIAN_POINT('Ctrl Pts',(-0.103266255382889,-0.150735748184266,
-0.354366953212811));
#36912=CARTESIAN_POINT('Ctrl Pts',(0.0688325172648546,-0.170265295386756,
-0.343414300764493));
#36913=CARTESIAN_POINT('Ctrl Pts',(0.180268213518661,-0.0350935526860387,
-0.332336420094669));
#36914=CARTESIAN_POINT('Ctrl Pts',(0.127677660483707,0.132009852885846,
-0.321258539424848));
#36915=CARTESIAN_POINT('Ctrl Pts',(-0.0410869387683269,0.178997345541052,
-0.310180658755025));
#36916=CARTESIAN_POINT('Ctrl Pts',(-0.144124030240022,0.0881142143007613,
-0.301492604759952));
#36917=CARTESIAN_POINT('Ctrl Pts',(-0.155502498570681,0.0183419554515344,
-0.296497177654821));
#36918=CARTESIAN_POINT('Ctrl Pts',(-0.155384523600718,0.000108282706206955,
-0.29519437743963));
#36919=CARTESIAN_POINT('Origin',(0.,0.,-0.90400562256037));
#36920=CARTESIAN_POINT('',(-0.155346404813911,8.48772195699003E-5,-0.44900562256037));
#36921=CARTESIAN_POINT('',(-0.155471787680923,-0.000134750021813443,-0.43519437743963));
#36922=CARTESIAN_POINT('',(-0.15555,-8.39731161192283E-15,-0.90400562256037));
#36923=CARTESIAN_POINT('Ctrl Pts',(-0.155346404813911,8.48772195699028E-5,
-0.44900562256037));
#36924=CARTESIAN_POINT('Ctrl Pts',(-0.155189329744259,-0.0313878464499768,
-0.446758275008691));
#36925=CARTESIAN_POINT('Ctrl Pts',(-0.130644203207247,-0.114798780034182,
-0.440818300567071));
#36926=CARTESIAN_POINT('Ctrl Pts',(0.00527308248792088,-0.183576646798727,
-0.431185699235508));
#36927=CARTESIAN_POINT('Ctrl Pts',(0.15678546817529,-0.0956373756302127,
-0.420107818565687));
#36928=CARTESIAN_POINT('Ctrl Pts',(0.165638580847071,0.079322450689304,
-0.409029937895864));
#36929=CARTESIAN_POINT('Ctrl Pts',(0.023776963372566,0.182106690325406,
-0.397952057226042));
#36930=CARTESIAN_POINT('Ctrl Pts',(-0.123930728671449,0.125267447494704,
-0.38794395211421));
#36931=CARTESIAN_POINT('Ctrl Pts',(-0.155161147300025,0.0365271619785578,
-0.38162847389232));
#36932=CARTESIAN_POINT('Ctrl Pts',(-0.155465071756645,-0.000133606378324543,
-0.37900562256037));
#36933=CARTESIAN_POINT('Ctrl Pts',(-0.155471787680923,-0.000134750021813448,
-0.43519437743963));
#36934=CARTESIAN_POINT('Ctrl Pts',(-0.155595181194392,-0.0148422151223725,
-0.434142033667443));
#36935=CARTESIAN_POINT('Ctrl Pts',(-0.146947534876927,-0.0810153094256527,
-0.429397063005316));
#36936=CARTESIAN_POINT('Ctrl Pts',(-0.0530564558970885,-0.175821496790065,
-0.420959465453248));
#36937=CARTESIAN_POINT('Ctrl Pts',(0.11849103787925,-0.140314148210727,
-0.409881584783426));
#36938=CARTESIAN_POINT('Ctrl Pts',(0.182223403637476,0.0228652009081741,
-0.398803704113603));
#36939=CARTESIAN_POINT('Ctrl Pts',(0.0801504904255299,0.165239478122968,
-0.387725823443781));
#36940=CARTESIAN_POINT('Ctrl Pts',(-0.0948514437538827,0.15726216920691,
-0.376647942773958));
#36941=CARTESIAN_POINT('Ctrl Pts',(-0.154985099422088,0.0548408623920629,
-0.369137460772575));
#36942=CARTESIAN_POINT('Ctrl Pts',(-0.155798217904179,0.00177257183384377,
-0.365319605661132));
#36943=CARTESIAN_POINT('Ctrl Pts',(-0.155793338978167,3.1743077477449E-5,
-0.36519437743963));
#36944=CARTESIAN_POINT('Origin',(0.,0.,-0.90400562256037));
#36945=CARTESIAN_POINT('',(-0.155766976288708,6.54450248024079E-5,-0.51900562256037));
#36946=CARTESIAN_POINT('',(-0.155342420051734,8.16789539274873E-5,-0.50519437743963));
#36947=CARTESIAN_POINT('',(-0.15555,-8.39731161192283E-15,-0.90400562256037));
#36948=CARTESIAN_POINT('Ctrl Pts',(-0.155766976288708,6.54450248024148E-5,
-0.51900562256037));
#36949=CARTESIAN_POINT('Ctrl Pts',(-0.155513327568197,-0.0475667116816575,
-0.515580703015002));
#36950=CARTESIAN_POINT('Ctrl Pts',(-0.106744701507368,-0.147003556334546,
-0.508463156579693));
#36951=CARTESIAN_POINT('Ctrl Pts',(0.0622509536759654,-0.172780234487164,
-0.497652983254442));
#36952=CARTESIAN_POINT('Ctrl Pts',(0.178789470703585,-0.0419823273947417,
-0.48657510258462));
#36953=CARTESIAN_POINT('Ctrl Pts',(0.132647248167164,0.127015346310585,
-0.475497221914797));
#36954=CARTESIAN_POINT('Ctrl Pts',(-0.0341908539685392,0.180441614256847,
-0.464419341244976));
#36955=CARTESIAN_POINT('Ctrl Pts',(-0.142383830605297,0.0921530609529823,
-0.455588808126832));
#36956=CARTESIAN_POINT('Ctrl Pts',(-0.15544742049907,0.0203251276447392,
-0.450450901898631));
#36957=CARTESIAN_POINT('Ctrl Pts',(-0.155346404813911,8.48772195699028E-5,
-0.44900562256037));
#36958=CARTESIAN_POINT('Ctrl Pts',(-0.155342420051734,8.16789539274786E-5,
-0.50519437743963));
#36959=CARTESIAN_POINT('Ctrl Pts',(-0.155192669039577,-0.0311489244921932,
-0.502964461673755));
#36960=CARTESIAN_POINT('Ctrl Pts',(-0.130936243323583,-0.114309881666503,
-0.497041919017939));
#36961=CARTESIAN_POINT('Ctrl Pts',(0.00441131476189927,-0.183599364242272,
-0.487426749472182));
#36962=CARTESIAN_POINT('Ctrl Pts',(0.156334808549674,-0.0963722671792685,
-0.47634886880236));
#36963=CARTESIAN_POINT('Ctrl Pts',(0.166009085015979,0.0785440636680758,
-0.465270988132537));
#36964=CARTESIAN_POINT('Ctrl Pts',(0.0246315091798845,0.18199306305922,
-0.454193107462715));
#36965=CARTESIAN_POINT('Ctrl Pts',(-0.123599083728466,0.12574999846804,
-0.444167570565079));
#36966=CARTESIAN_POINT('Ctrl Pts',(-0.15516219891434,0.0367656173641079,
-0.437834660557384));
#36967=CARTESIAN_POINT('Ctrl Pts',(-0.155471787680923,-0.000134750021813448,
-0.43519437743963));
#36968=CARTESIAN_POINT('Origin',(0.,0.,-0.90400562256037));
#36969=CARTESIAN_POINT('',(-0.155529154618988,-0.000139780194698154,-0.58900562256037));
#36970=CARTESIAN_POINT('',(-0.155762681169959,6.92827665681687E-5,-0.57519437743963));
#36971=CARTESIAN_POINT('',(-0.15555,-8.39731161192283E-15,-0.90400562256037));
#36972=CARTESIAN_POINT('Ctrl Pts',(-0.155529154618988,-0.000139780194698135,
-0.58900562256037));
#36973=CARTESIAN_POINT('Ctrl Pts',(-0.155643250350289,-0.0128440365105712,
-0.588095757911254));
#36974=CARTESIAN_POINT('Ctrl Pts',(-0.148424039982469,-0.0769797460374569,
-0.583493266372197));
#36975=CARTESIAN_POINT('Ctrl Pts',(-0.0597614480239172,-0.173657013877139,
-0.575198147943198));
#36976=CARTESIAN_POINT('Ctrl Pts',(0.113021777413197,-0.144755894581878,
-0.564120267273377));
#36977=CARTESIAN_POINT('Ctrl Pts',(0.182966362384724,0.0158587828225596,
-0.553042386603554));
#36978=CARTESIAN_POINT('Ctrl Pts',(0.0864296486912397,0.162043532007437,
-0.541964505933732));
#36979=CARTESIAN_POINT('Ctrl Pts',(-0.0887494987382724,0.160784692096253,
-0.53088662526391));
#36980=CARTESIAN_POINT('Ctrl Pts',(-0.15398197464732,0.0588474973592622,
-0.523233664139455));
#36981=CARTESIAN_POINT('Ctrl Pts',(-0.155786802630472,0.00378859180802485,
-0.519273329904942));
#36982=CARTESIAN_POINT('Ctrl Pts',(-0.155766976288708,6.54450248024148E-5,
-0.51900562256037));
#36983=CARTESIAN_POINT('Ctrl Pts',(-0.155762681169959,6.9282766568167E-5,
-0.575194377439629));
#36984=CARTESIAN_POINT('Ctrl Pts',(-0.155497913037279,-0.0473238951863867,
-0.571786889680066));
#36985=CARTESIAN_POINT('Ctrl Pts',(-0.10716124014269,-0.146543711339655,
-0.564686775030562));
#36986=CARTESIAN_POINT('Ctrl Pts',(0.0614392328065822,-0.173070526112361,
-0.553894033491116));
#36987=CARTESIAN_POINT('Ctrl Pts',(0.178590424220399,-0.0428211002752123,
-0.542816152821293));
#36988=CARTESIAN_POINT('Ctrl Pts',(0.133241988508851,0.126391292087037,
-0.531738272151472));
#36989=CARTESIAN_POINT('Ctrl Pts',(-0.0333434816106114,0.180600106574017,
-0.520660391481649));
#36990=CARTESIAN_POINT('Ctrl Pts',(-0.142164078467833,0.092647109507526,
-0.511812426577702));
#36991=CARTESIAN_POINT('Ctrl Pts',(-0.155440649085617,0.0205673635573518,
-0.506657088563695));
#36992=CARTESIAN_POINT('Ctrl Pts',(-0.155342420051734,8.16789539274786E-5,
-0.50519437743963));
#36993=CARTESIAN_POINT('Origin',(0.,0.,-0.90400562256037));
#36994=CARTESIAN_POINT('',(-0.155316084506021,5.35377555358372E-5,-0.659005622560371));
#36995=CARTESIAN_POINT('',(-0.155536374284098,-0.000139852232319077,-0.64519437743963));
#36996=CARTESIAN_POINT('',(-0.15555,-8.39731161192283E-15,-0.90400562256037));
#36997=CARTESIAN_POINT('Ctrl Pts',(-0.155316084506021,5.3537755535819E-5,
-0.65900562256037));
#36998=CARTESIAN_POINT('Ctrl Pts',(-0.155225416432192,-0.0291940910521941,
-0.656918185917565));
#36999=CARTESIAN_POINT('Ctrl Pts',(-0.133259818681327,-0.110306616722607,
-0.65113812238482));
#37000=CARTESIAN_POINT('Ctrl Pts',(-0.00263426887515189,-0.183633273387178,
-0.641665431962132));
#37001=CARTESIAN_POINT('Ctrl Pts',(0.15252317418251,-0.102298032825963,
-0.630587551292311));
#37002=CARTESIAN_POINT('Ctrl Pts',(0.168899673978284,0.0721186645451872,
-0.619509670622488));
#37003=CARTESIAN_POINT('Ctrl Pts',(0.0315941379137935,0.180914318189617,
-0.608431789952666));
#37004=CARTESIAN_POINT('Ctrl Pts',(-0.120820410002026,0.129680488142133,
-0.598263773931959));
#37005=CARTESIAN_POINT('Ctrl Pts',(-0.155180200196799,0.038715366895471,
-0.591788384801195));
#37006=CARTESIAN_POINT('Ctrl Pts',(-0.155529154618988,-0.000139780194698135,
-0.58900562256037));
#37007=CARTESIAN_POINT('Ctrl Pts',(-0.155536374284098,-0.000139852232319075,
-0.64519437743963));
#37008=CARTESIAN_POINT('Ctrl Pts',(-0.155648810427832,-0.0125992364466732,
-0.644301944576318));
#37009=CARTESIAN_POINT('Ctrl Pts',(-0.148598384175115,-0.0764862520907471,
-0.639716884823065));
#37010=CARTESIAN_POINT('Ctrl Pts',(-0.0605759234386941,-0.17337454580915,
-0.631439198179872));
#37011=CARTESIAN_POINT('Ctrl Pts',(0.112341035698075,-0.145284827074641,
-0.62036131751005));
#37012=CARTESIAN_POINT('Ctrl Pts',(0.183038778318879,0.0149997688499129,
-0.609283436840227));
#37013=CARTESIAN_POINT('Ctrl Pts',(0.0871893223770248,0.161636031852426,
-0.598205556170405));
#37014=CARTESIAN_POINT('Ctrl Pts',(-0.0879937907449659,0.161199502407392,
-0.587127675500583));
#37015=CARTESIAN_POINT('Ctrl Pts',(-0.153853711608356,0.0593381461278729,
-0.579457282590324));
#37016=CARTESIAN_POINT('Ctrl Pts',(-0.155784837010399,0.00403515161213462,
-0.575479516570006));
#37017=CARTESIAN_POINT('Ctrl Pts',(-0.155762681169959,6.9282766568167E-5,
-0.575194377439629));
#37018=CARTESIAN_POINT('Origin',(0.,0.,-0.90400562256037));
#37019=CARTESIAN_POINT('',(-0.155718793124499,0.000108222005882066,-0.72900562256037));
#37020=CARTESIAN_POINT('',(-0.155313284670072,5.07842058497104E-5,-0.71519437743963));
#37021=CARTESIAN_POINT('',(-0.15555,-8.39731161192283E-15,-0.90400562256037));
#37022=CARTESIAN_POINT('Ctrl Pts',(-0.155718793124499,0.000108222005882058,
-0.72900562256037));
#37023=CARTESIAN_POINT('Ctrl Pts',(-0.155384204900034,-0.0453333351310797,
-0.725740613923876));
#37024=CARTESIAN_POINT('Ctrl Pts',(-0.110495670244879,-0.142777587024444,
-0.718782978397442));
#37025=CARTESIAN_POINT('Ctrl Pts',(0.0547571568913644,-0.175290438141162,
-0.708132715981067));
#37026=CARTESIAN_POINT('Ctrl Pts',(0.176815643105561,-0.0496447546162005,
-0.697054835311244));
#37027=CARTESIAN_POINT('Ctrl Pts',(0.137992423121185,0.121190070497784,
-0.685976954641421));
#37028=CARTESIAN_POINT('Ctrl Pts',(-0.0263918556098016,0.181744822170133,
-0.6748990739716));
#37029=CARTESIAN_POINT('Ctrl Pts',(-0.140311098627796,0.0966842315348642,
-0.665908629944582));
#37030=CARTESIAN_POINT('Ctrl Pts',(-0.155385806146838,0.0225442843254148,
-0.660610812807506));
#37031=CARTESIAN_POINT('Ctrl Pts',(-0.155316084506021,5.3537755535819E-5,
-0.65900562256037));
#37032=CARTESIAN_POINT('Ctrl Pts',(-0.155313284670072,5.07842058496948E-5,
-0.71519437743963));
#37033=CARTESIAN_POINT('Ctrl Pts',(-0.155229832237143,-0.0289541923389479,
-0.713124372582629));
#37034=CARTESIAN_POINT('Ctrl Pts',(-0.133537000198005,-0.109817572601608,
-0.707361740835688));
#37035=CARTESIAN_POINT('Ctrl Pts',(-0.00349579444440964,-0.183617766674194,
-0.697906482198806));
#37036=CARTESIAN_POINT('Ctrl Pts',(0.152041075972361,-0.103013424219718,
-0.686828601528983));
#37037=CARTESIAN_POINT('Ctrl Pts',(0.169236443271834,0.0713253547488333,
-0.675750720859162));
#37038=CARTESIAN_POINT('Ctrl Pts',(0.0324429392663866,0.18076385018324,
-0.664672840189339));
#37039=CARTESIAN_POINT('Ctrl Pts',(-0.120472031008651,0.130159640264286,
-0.654487392382829));
#37040=CARTESIAN_POINT('Ctrl Pts',(-0.155183582459629,0.0389540613681267,
-0.647994571466259));
#37041=CARTESIAN_POINT('Ctrl Pts',(-0.155536374284098,-0.000139852232319075,
-0.64519437743963));
#37042=CARTESIAN_POINT('Ctrl Pts',(-0.0685825729128701,0.139614588036676,
-0.797607408227207));
#37043=CARTESIAN_POINT('Ctrl Pts',(-0.114857746382803,0.116882934395126,
-0.793914781337266));
#37044=CARTESIAN_POINT('Ctrl Pts',(-0.182252520735991,0.0222053183358603,
-0.786529527557385));
#37045=CARTESIAN_POINT('Ctrl Pts',(-0.117832146183986,-0.141024052804591,
-0.775451646887562));
#37046=CARTESIAN_POINT('Ctrl Pts',(0.0539538561217182,-0.175492392417165,
-0.764373766217739));
#37047=CARTESIAN_POINT('Ctrl Pts',(0.176570107319903,-0.0505019485347378,
-0.753295885547919));
#37048=CARTESIAN_POINT('Ctrl Pts',(0.138565293653093,0.120555556476704,
-0.742218004878094));
#37049=CARTESIAN_POINT('Ctrl Pts',(-0.0255413571731973,0.181859045827175,
-0.731140124208274));
#37050=CARTESIAN_POINT('Ctrl Pts',(-0.166396812434887,0.0777204685530644,
-0.72006224353845));
#37051=CARTESIAN_POINT('Ctrl Pts',(-0.155853441635454,-0.0971526815038287,
-0.708984362868629));
#37052=CARTESIAN_POINT('Ctrl Pts',(-0.00349579444440964,-0.183617766674194,
-0.697906482198806));
#37053=CARTESIAN_POINT('Ctrl Pts',(0.152041075972361,-0.103013424219718,
-0.686828601528983));
#37054=CARTESIAN_POINT('Ctrl Pts',(0.169236443271834,0.0713253547488333,
-0.675750720859162));
#37055=CARTESIAN_POINT('Ctrl Pts',(0.0324429392663866,0.18076385018324,
-0.664672840189339));
#37056=CARTESIAN_POINT('Ctrl Pts',(-0.133870199391445,0.125725779248893,
-0.653594959519517));
#37057=CARTESIAN_POINT('Ctrl Pts',(-0.17837481560913,-0.0437106671942546,
-0.642517078849694));
#37058=CARTESIAN_POINT('Ctrl Pts',(-0.0605759234386941,-0.17337454580915,
-0.631439198179872));
#37059=CARTESIAN_POINT('Ctrl Pts',(0.112341035698075,-0.145284827074641,
-0.62036131751005));
#37060=CARTESIAN_POINT('Ctrl Pts',(0.183038778318879,0.0149997688499129,
-0.609283436840227));
#37061=CARTESIAN_POINT('Ctrl Pts',(0.0871893223770248,0.161636031852426,
-0.598205556170405));
#37062=CARTESIAN_POINT('Ctrl Pts',(-0.0879937907449659,0.161199502407392,
-0.587127675500583));
#37063=CARTESIAN_POINT('Ctrl Pts',(-0.18311125770977,0.0140873579667044,
-0.57604979483076));
#37064=CARTESIAN_POINT('Ctrl Pts',(-0.111615584950465,-0.145842885431028,
-0.564971914160939));
#37065=CARTESIAN_POINT('Ctrl Pts',(0.0614392328065822,-0.173070526112361,
-0.553894033491116));
#37066=CARTESIAN_POINT('Ctrl Pts',(0.178590424220399,-0.0428211002752123,
-0.542816152821293));
#37067=CARTESIAN_POINT('Ctrl Pts',(0.133241988508851,0.126391292087037,
-0.531738272151472));
#37068=CARTESIAN_POINT('Ctrl Pts',(-0.0333434816106114,0.180600106574017,
-0.520660391481649));
#37069=CARTESIAN_POINT('Ctrl Pts',(-0.169589680537707,0.0704806817533824,
-0.509582510811826));
#37070=CARTESIAN_POINT('Ctrl Pts',(-0.1515260392585,-0.103769194218193,
-0.498504630142005));
#37071=CARTESIAN_POINT('Ctrl Pts',(0.00441131476189927,-0.183599364242272,
-0.487426749472182));
#37072=CARTESIAN_POINT('Ctrl Pts',(0.156334808549674,-0.0963722671792685,
-0.47634886880236));
#37073=CARTESIAN_POINT('Ctrl Pts',(0.166009085015979,0.0785440636680758,
-0.465270988132537));
#37074=CARTESIAN_POINT('Ctrl Pts',(0.0246315091798845,0.18199306305922,
-0.454193107462715));
#37075=CARTESIAN_POINT('Ctrl Pts',(-0.139158304435279,0.119846370626905,
-0.443115226792893));
#37076=CARTESIAN_POINT('Ctrl Pts',(-0.17632782105536,-0.0513486686061268,
-0.43203734612307));
#37077=CARTESIAN_POINT('Ctrl Pts',(-0.0530564558970885,-0.175821496790065,
-0.420959465453248));
#37078=CARTESIAN_POINT('Ctrl Pts',(0.11849103787925,-0.140314148210727,
-0.409881584783426));
#37079=CARTESIAN_POINT('Ctrl Pts',(0.182223403637476,0.0228652009081741,
-0.398803704113603));
#37080=CARTESIAN_POINT('Ctrl Pts',(0.0801504904255299,0.165239478122968,
-0.387725823443781));
#37081=CARTESIAN_POINT('Ctrl Pts',(-0.0948514437538827,0.15726216920691,
-0.376647942773958));
#37082=CARTESIAN_POINT('Ctrl Pts',(-0.183547943074409,0.00619183647286117,
-0.365570062104137));
#37083=CARTESIAN_POINT('Ctrl Pts',(-0.105233963508669,-0.150512455198895,
-0.354492181434313));
#37084=CARTESIAN_POINT('Ctrl Pts',(0.0688325172648546,-0.170265295386756,
-0.343414300764493));
#37085=CARTESIAN_POINT('Ctrl Pts',(0.180268213518661,-0.0350935526860387,
-0.332336420094669));
#37086=CARTESIAN_POINT('Ctrl Pts',(0.127677660483707,0.132009852885846,
-0.321258539424848));
#37087=CARTESIAN_POINT('Ctrl Pts',(-0.0410869387683269,0.178997345541052,
-0.310180658755025));
#37088=CARTESIAN_POINT('Ctrl Pts',(-0.172466486424957,0.0631149530800074,
-0.299102778085203));
#37089=CARTESIAN_POINT('Ctrl Pts',(-0.146918585030578,-0.110195805809095,
-0.28802489741538));
#37090=CARTESIAN_POINT('Ctrl Pts',(0.0123107014066272,-0.183239277698152,
-0.276947016745558));
#37091=CARTESIAN_POINT('Ctrl Pts',(0.160338466762532,-0.0895531255371017,
-0.265869136075736));
#37092=CARTESIAN_POINT('Ctrl Pts',(0.162474081881463,0.0856175155489654,
-0.254791255405913));
#37093=CARTESIAN_POINT('Ctrl Pts',(0.0167743476807649,0.182884683876359,
-0.243713374736091));
#37094=CARTESIAN_POINT('Ctrl Pts',(-0.144188383635275,0.113744872672702,
-0.232635494066269));
#37095=CARTESIAN_POINT('Ctrl Pts',(-0.173953944439453,-0.0588915237406155,
-0.221557613396446));
#37096=CARTESIAN_POINT('Ctrl Pts',(-0.045438614211677,-0.177942460150977,
-0.210479732726624));
#37097=CARTESIAN_POINT('Ctrl Pts',(0.124421357682504,-0.135083346427328,
-0.199401852056802));
#37098=CARTESIAN_POINT('Ctrl Pts',(0.181070205071097,0.0306882431808897,
-0.18832397138698));
#37099=CARTESIAN_POINT('Ctrl Pts',(0.0729630546502829,0.168536589309041,
-0.177246090717157));
#37100=CARTESIAN_POINT('Ctrl Pts',(-0.1015332313447,0.153033259678028,-0.166168210047335));
#37101=CARTESIAN_POINT('Ctrl Pts',(-0.183644372729135,-0.0017151195528544,
-0.155090329377512));
#37102=CARTESIAN_POINT('Ctrl Pts',(-0.0986571866185378,-0.154903070922954,
-0.14401244870769));
#37103=CARTESIAN_POINT('Ctrl Pts',(0.0760980799328472,-0.16714423732766,
-0.132934568037868));
#37104=CARTESIAN_POINT('Ctrl Pts',(0.181612007146477,-0.027301260439323,
-0.121856687368045));
#37105=CARTESIAN_POINT('Ctrl Pts',(0.121876225192118,0.137384278886722,
-0.110778806698223));
#37106=CARTESIAN_POINT('Ctrl Pts',(-0.0487534599252984,0.177061585225392,
-0.0997009260284008));
#37107=CARTESIAN_POINT('Ctrl Pts',(-0.175025004118839,0.0556344023622128,
-0.0886230453585786));
#37108=CARTESIAN_POINT('Ctrl Pts',(-0.142035983272133,-0.116422291149579,
-0.0775451646887562));
#37109=CARTESIAN_POINT('Ctrl Pts',(0.0201819892413759,-0.182531533674816,
-0.0664672840189338));
#37110=CARTESIAN_POINT('Ctrl Pts',(0.164054917332699,-0.0825830908935778,
-0.0553894033491116));
#37111=CARTESIAN_POINT('Ctrl Pts',(0.158618708021993,0.0925610883157775,
-0.0443115226792891));
#37112=CARTESIAN_POINT('Ctrl Pts',(0.00892266599271826,0.183382072237952,
-0.0332336420094669));
#37113=CARTESIAN_POINT('Ctrl Pts',(-0.149021641743064,0.107539520344655,
-0.0221557613396447));
#37114=CARTESIAN_POINT('Ctrl Pts',(-0.171116143090106,-0.0665456463713913,
-0.0110778806698222));
#37115=CARTESIAN_POINT('Ctrl Pts',(-0.0824189364736414,-0.141637004936936,
-0.00369262688994078));
#37116=CARTESIAN_POINT('Ctrl Pts',(-0.0319621170202007,-0.152230829911641,
0.));
#37117=CARTESIAN_POINT('Ctrl Pts',(-0.0744392439309299,0.151537102412036,
-0.789938272151471));
#37118=CARTESIAN_POINT('Ctrl Pts',(-0.124666127810757,0.126864258590232,
-0.786245645261531));
#37119=CARTESIAN_POINT('Ctrl Pts',(-0.197816140046672,0.024101561635302,
-0.778860391481648));
#37120=CARTESIAN_POINT('Ctrl Pts',(-0.127894529180734,-0.153066929702187,
-0.767782510811827));
#37121=CARTESIAN_POINT('Ctrl Pts',(0.0585612946011998,-0.190478724438646,
-0.756704630142004));
#37122=CARTESIAN_POINT('Ctrl Pts',(0.191648471782987,-0.0548146082349622,
-0.745626749472183));
#37123=CARTESIAN_POINT('Ctrl Pts',(0.15039820258286,0.130850507565521,-0.734548868802359));
#37124=CARTESIAN_POINT('Ctrl Pts',(-0.0277224845349277,0.197389063991137,
-0.723470988132538));
#37125=CARTESIAN_POINT('Ctrl Pts',(-0.18060641915412,0.084357478457361,
-0.712393107462715));
#37126=CARTESIAN_POINT('Ctrl Pts',(-0.169162687642468,-0.105449122858007,
-0.701315226792893));
#37127=CARTESIAN_POINT('Ctrl Pts',(-0.00379432098166487,-0.199297972400041,
-0.690237346123071));
#37128=CARTESIAN_POINT('Ctrl Pts',(0.165024761555771,-0.111810349013795,
-0.679159465453248));
#37129=CARTESIAN_POINT('Ctrl Pts',(0.183688542841925,0.077416248109469,
-0.668081584783426));
#37130=CARTESIAN_POINT('Ctrl Pts',(0.0352134334906785,0.196200343121849,
-0.657003704113603));
#37131=CARTESIAN_POINT('Ctrl Pts',(-0.145302166488303,0.136462246200717,
-0.645925823443781));
#37132=CARTESIAN_POINT('Ctrl Pts',(-0.193607294773437,-0.0474433792647373,
-0.634847942773958));
#37133=CARTESIAN_POINT('Ctrl Pts',(-0.0657488593629036,-0.188180022398659,
-0.623770062104138));
#37134=CARTESIAN_POINT('Ctrl Pts',(0.121934500334457,-0.157691556655536,
-0.612692181434313));
#37135=CARTESIAN_POINT('Ctrl Pts',(0.198669540808984,0.016280687715591,
-0.601614300764494));
#37136=CARTESIAN_POINT('Ctrl Pts',(0.0946349336418375,0.175439087395807,
-0.590536420094668));
#37137=CARTESIAN_POINT('Ctrl Pts',(-0.0955081003157075,0.174965280122885,
-0.579458539424848));
#37138=CARTESIAN_POINT('Ctrl Pts',(-0.198748209643198,0.0152903606774588,
-0.568380658755025));
#37139=CARTESIAN_POINT('Ctrl Pts',(-0.121147099062276,-0.158297270911422,
-0.557302778085202));
#37140=CARTESIAN_POINT('Ctrl Pts',(0.0666858918172795,-0.187850040664119,
-0.546224897415381));
#37141=CARTESIAN_POINT('Ctrl Pts',(0.193841315477621,-0.0464778469718106,
-0.535147016745557));
#37142=CARTESIAN_POINT('Ctrl Pts',(0.144620308967606,0.137184591111291,
-0.524069136075737));
#37143=CARTESIAN_POINT('Ctrl Pts',(-0.0361908784651756,0.196022616478603,
-0.512991255405913));
#37144=CARTESIAN_POINT('Ctrl Pts',(-0.184071945124501,0.0764994434974575,
-0.501913374736091));
#37145=CARTESIAN_POINT('Ctrl Pts',(-0.164465742814594,-0.11263065867677,
-0.490835494066269));
#37146=CARTESIAN_POINT('Ctrl Pts',(0.00478802298703869,-0.199277998475755,
-0.479757613396446));
#37147=CARTESIAN_POINT('Ctrl Pts',(0.169685161320925,-0.104602064344369,
-0.468679732726624));
#37148=CARTESIAN_POINT('Ctrl Pts',(0.180185581400608,0.0852514052242152,
-0.457601852056802));
#37149=CARTESIAN_POINT('Ctrl Pts',(0.0267349392469986,0.197534525746265,
-0.446523971386979));
#37150=CARTESIAN_POINT('Ctrl Pts',(-0.151041854058649,0.13008076014685,
-0.435446090717158));
#37151=CARTESIAN_POINT('Ctrl Pts',(-0.191385495263131,-0.0557336347348181,
-0.424368210047334));
#37152=CARTESIAN_POINT('Ctrl Pts',(-0.0575872600704507,-0.190835932977966,
-0.413290329377513));
#37153=CARTESIAN_POINT('Ctrl Pts',(0.128609687529926,-0.152296402161649,
-0.40221244870769));
#37154=CARTESIAN_POINT('Ctrl Pts',(0.19778453646712,0.0248177954783882,
-0.391134568037868));
#37155=CARTESIAN_POINT('Ctrl Pts',(0.0869950142516475,0.179350253228936,
-0.380056687368046));
#37156=CARTESIAN_POINT('Ctrl Pts',(-0.102951368823189,0.170691714782599,
-0.368978806698223));
#37157=CARTESIAN_POINT('Ctrl Pts',(-0.199222186150622,0.00672059396443702,
-0.357900926028401));
#37158=CARTESIAN_POINT('Ctrl Pts',(-0.114220513269348,-0.163365602824901,
-0.346823045358578));
#37159=CARTESIAN_POINT('Ctrl Pts',(0.0747105325075507,-0.184805254716366,
-0.335745164688756));
#37160=CARTESIAN_POINT('Ctrl Pts',(0.195662381114758,-0.0380903984473996,
-0.324667284018934));
#37161=CARTESIAN_POINT('Ctrl Pts',(0.138580810103928,0.143282954005531,
-0.313589403349111));
#37162=CARTESIAN_POINT('Ctrl Pts',(-0.0445955951701644,0.194282986213528,
-0.30251152267929));
#37163=CARTESIAN_POINT('Ctrl Pts',(-0.187194418459746,0.0685047117433281,
-0.291433642009467));
#37164=CARTESIAN_POINT('Ctrl Pts',(-0.159464830853934,-0.119606076593391,
-0.280355761339645));
#37165=CARTESIAN_POINT('Ctrl Pts',(0.0133619849190106,-0.198887162014602,
-0.269277880669822));
#37166=CARTESIAN_POINT('Ctrl Pts',(0.174030715558174,-0.0972005959167307,
-0.2582));
#37167=CARTESIAN_POINT('Ctrl Pts',(0.176348703467184,0.0929289009440708,
-0.247122119330178));
#37168=CARTESIAN_POINT('Ctrl Pts',(0.0182068083152422,0.198502287331782,
-0.236044238660356));
#37169=CARTESIAN_POINT('Ctrl Pts',(-0.156501481434194,0.12345821924081,
-0.224966357990533));
#37170=CARTESIAN_POINT('Ctrl Pts',(-0.18880889930051,-0.063920618824861,
-0.213888477320711));
#37171=CARTESIAN_POINT('Ctrl Pts',(-0.049318885884956,-0.19313801792879,
-0.202810596650889));
#37172=CARTESIAN_POINT('Ctrl Pts',(0.135046432371559,-0.146618911315637,
-0.191732715981066));
#37173=CARTESIAN_POINT('Ctrl Pts',(0.196532859463218,0.0333088935414555,
-0.180654835311244));
#37174=CARTESIAN_POINT('Ctrl Pts',(0.0791938008793927,0.182928924215213,
-0.169576954641422));
#37175=CARTESIAN_POINT('Ctrl Pts',(-0.110203753725683,0.166101673688893,
-0.158499073971599));
#37176=CARTESIAN_POINT('Ctrl Pts',(-0.199326850503175,-0.00186158374267733,
-0.147421193301777));
#37177=CARTESIAN_POINT('Ctrl Pts',(-0.107082106551569,-0.16813115916099,
-0.136343312631954));
#37178=CARTESIAN_POINT('Ctrl Pts',(0.0825965444894176,-0.181417671073524,
-0.125265431962133));
#37179=CARTESIAN_POINT('Ctrl Pts',(0.197120929218237,-0.0296326763366925,
-0.11418755129231));
#37180=CARTESIAN_POINT('Ctrl Pts',(0.132283955983731,0.149116333989338,
-0.103109670622488));
#37181=CARTESIAN_POINT('Ctrl Pts',(-0.0529168058548446,0.192181919889984,
-0.0920317899526653));
#37182=CARTESIAN_POINT('Ctrl Pts',(-0.189971423092665,0.060385352612153,
-0.080953909282843));
#37183=CARTESIAN_POINT('Ctrl Pts',(-0.154165274889822,-0.126364278296928,
-0.0698760286130208));
#37184=CARTESIAN_POINT('Ctrl Pts',(0.0219054485176395,-0.198118979548471,
-0.0587981479431983));
#37185=CARTESIAN_POINT('Ctrl Pts',(0.178064535795589,-0.0896353488430248,
-0.047720267273376));
#37186=CARTESIAN_POINT('Ctrl Pts',(0.172164096460172,0.100465426405102,
-0.0366423866035536));
#37187=CARTESIAN_POINT('Ctrl Pts',(0.0096846251479957,0.199042150623642,
-0.0255645059337314));
#37188=CARTESIAN_POINT('Ctrl Pts',(-0.161747480001847,0.116722955222475,
-0.0144866252639091));
#37189=CARTESIAN_POINT('Ctrl Pts',(-0.185728761331059,-0.0722283721999558,
-0.00340874459408669));
#37190=CARTESIAN_POINT('Ctrl Pts',(-0.0894571763075103,-0.153732225437818,
0.00397650918579475));
#37191=CARTESIAN_POINT('Ctrl Pts',(-0.0346915509926754,-0.165230719704803,
0.00766913607573553));
#37192=CARTESIAN_POINT('Ctrl Pts',(-0.0802959149489896,0.163459616787396,
-0.782269136075736));
#37193=CARTESIAN_POINT('Ctrl Pts',(-0.13447450923871,0.136845582785338,
-0.778576509185795));
#37194=CARTESIAN_POINT('Ctrl Pts',(-0.213379759357353,0.0259978049347435,
-0.771191255405914));
#37195=CARTESIAN_POINT('Ctrl Pts',(-0.137956912177481,-0.165109806599782,
-0.760113374736091));
#37196=CARTESIAN_POINT('Ctrl Pts',(0.0631687330806816,-0.205465056460127,
-0.749035494066269));
#37197=CARTESIAN_POINT('Ctrl Pts',(0.20672683624607,-0.0591272679351864,
-0.737957613396446));
#37198=CARTESIAN_POINT('Ctrl Pts',(0.162231111512628,0.141145458654337,
-0.726879732726624));
#37199=CARTESIAN_POINT('Ctrl Pts',(-0.0299036118966582,0.212919082155099,
-0.715801852056802));
#37200=CARTESIAN_POINT('Ctrl Pts',(-0.194816025873353,0.0909944883616574,
-0.704723971386979));
#37201=CARTESIAN_POINT('Ctrl Pts',(-0.182471933649482,-0.113745564212185,
-0.693646090717158));
#37202=CARTESIAN_POINT('Ctrl Pts',(-0.00409284751891995,-0.214978178125889,
-0.682568210047334));
#37203=CARTESIAN_POINT('Ctrl Pts',(0.178008447139181,-0.120607273807872,
-0.671490329377513));
#37204=CARTESIAN_POINT('Ctrl Pts',(0.198140642412015,0.0835071414701047,
-0.66041244870769));
#37205=CARTESIAN_POINT('Ctrl Pts',(0.0379839277149706,0.211636836060458,
-0.649334568037868));
#37206=CARTESIAN_POINT('Ctrl Pts',(-0.156734133585161,0.147198713152541,
-0.638256687368046));
#37207=CARTESIAN_POINT('Ctrl Pts',(-0.208839773937744,-0.0511760913352197,
-0.627178806698223));
#37208=CARTESIAN_POINT('Ctrl Pts',(-0.0709217952871131,-0.202985498988168,
-0.616100926028401));
#37209=CARTESIAN_POINT('Ctrl Pts',(0.13152796497084,-0.170098286236431,
-0.605023045358579));
#37210=CARTESIAN_POINT('Ctrl Pts',(0.214300303299088,0.0175616065812689,
-0.593945164688756));
#37211=CARTESIAN_POINT('Ctrl Pts',(0.10208054490665,0.189242142939189,-0.582867284018934));
#37212=CARTESIAN_POINT('Ctrl Pts',(-0.103022409886449,0.188731057838378,
-0.571789403349112));
#37213=CARTESIAN_POINT('Ctrl Pts',(-0.214385161576627,0.0164933633882133,
-0.560711522679289));
#37214=CARTESIAN_POINT('Ctrl Pts',(-0.130678613174086,-0.170751656391817,
-0.549633642009467));
#37215=CARTESIAN_POINT('Ctrl Pts',(0.0719325508279769,-0.202629555215876,
-0.538555761339645));
#37216=CARTESIAN_POINT('Ctrl Pts',(0.209092206734844,-0.050134593668409,
-0.527477880669822));
#37217=CARTESIAN_POINT('Ctrl Pts',(0.155998629426361,0.147977890135545,
-0.5164));
#37218=CARTESIAN_POINT('Ctrl Pts',(-0.0390382753197402,0.211445126383187,
-0.505322119330178));
#37219=CARTESIAN_POINT('Ctrl Pts',(-0.198554209711295,0.0825182052415327,
-0.494244238660355));
#37220=CARTESIAN_POINT('Ctrl Pts',(-0.177405446370688,-0.121492123135346,
-0.483166357990533));
#37221=CARTESIAN_POINT('Ctrl Pts',(0.00516473121217803,-0.214956632709237,
-0.472088477320711));
#37222=CARTESIAN_POINT('Ctrl Pts',(0.183035514092176,-0.11283186150947,
-0.461010596650888));
#37223=CARTESIAN_POINT('Ctrl Pts',(0.194362077785237,0.0919587467803548,
-0.449932715981067));
#37224=CARTESIAN_POINT('Ctrl Pts',(0.0288383693141127,0.213075988433311,
-0.438854835311244));
#37225=CARTESIAN_POINT('Ctrl Pts',(-0.162925403682019,0.140315149666796,
-0.427776954641422));
#37226=CARTESIAN_POINT('Ctrl Pts',(-0.206443169470902,-0.0601186008635093,
-0.416699073971599));
#37227=CARTESIAN_POINT('Ctrl Pts',(-0.0621180642438127,-0.205850369165867,
-0.405621193301777));
#37228=CARTESIAN_POINT('Ctrl Pts',(0.138728337180602,-0.164278656112571,
-0.394543312631955));
#37229=CARTESIAN_POINT('Ctrl Pts',(0.213345669296764,0.0267703900486021,
-0.383465431962132));
#37230=CARTESIAN_POINT('Ctrl Pts',(0.093839538077765,0.193461028334904,
-0.37238755129231));
#37231=CARTESIAN_POINT('Ctrl Pts',(-0.111051293892496,0.184121260358289,
-0.361309670622487));
#37232=CARTESIAN_POINT('Ctrl Pts',(-0.214896429226836,0.00724935145601278,
-0.350231789952666));
#37233=CARTESIAN_POINT('Ctrl Pts',(-0.123207063030027,-0.176218750450907,
-0.339153909282843));
#37234=CARTESIAN_POINT('Ctrl Pts',(0.0805885477502469,-0.199345214045976,
-0.328076028613021));
#37235=CARTESIAN_POINT('Ctrl Pts',(0.211056548710855,-0.0410872442087603,
-0.316998147943199));
#37236=CARTESIAN_POINT('Ctrl Pts',(0.149483959724149,0.154556055125215,
-0.305920267273376));
#37237=CARTESIAN_POINT('Ctrl Pts',(-0.048104251572002,0.209568626886004,
-0.294842386603554));
#37238=CARTESIAN_POINT('Ctrl Pts',(-0.201922350494536,0.073894470406649,
-0.283764505933731));
#37239=CARTESIAN_POINT('Ctrl Pts',(-0.172011076677289,-0.129016347377688,
-0.272686625263909));
#37240=CARTESIAN_POINT('Ctrl Pts',(0.014413268431394,-0.214535046331052,
-0.261608744594087));
#37241=CARTESIAN_POINT('Ctrl Pts',(0.187722964353817,-0.10484806629636,
-0.250530863924265));
#37242=CARTESIAN_POINT('Ctrl Pts',(0.190223325052905,0.100240286339176,
-0.239452983254442));
#37243=CARTESIAN_POINT('Ctrl Pts',(0.0196392689497196,0.214119890787204,
-0.22837510258462));
#37244=CARTESIAN_POINT('Ctrl Pts',(-0.168814579233112,0.133171565808918,
-0.217297221914798));
#37245=CARTESIAN_POINT('Ctrl Pts',(-0.203663854161568,-0.0689497139091067,
-0.206219341244975));
#37246=CARTESIAN_POINT('Ctrl Pts',(-0.053199157558235,-0.208333575706603,
-0.195141460575153));
#37247=CARTESIAN_POINT('Ctrl Pts',(0.145671507060614,-0.158154476203945,
-0.184063579905331));
#37248=CARTESIAN_POINT('Ctrl Pts',(0.211995513855339,0.0359295439020216,
-0.172985699235508));
#37249=CARTESIAN_POINT('Ctrl Pts',(0.0854245471085026,0.197321259121385,
-0.161907818565686));
#37250=CARTESIAN_POINT('Ctrl Pts',(-0.118874276106667,0.179170087699757,
-0.150829937895864));
#37251=CARTESIAN_POINT('Ctrl Pts',(-0.215009328277216,-0.00200804793250031,
-0.139752057226041));
#37252=CARTESIAN_POINT('Ctrl Pts',(-0.1155070264846,-0.181359247399026,
-0.128674176556219));
#37253=CARTESIAN_POINT('Ctrl Pts',(0.0890950090459882,-0.195691104819388,
-0.117596295886397));
#37254=CARTESIAN_POINT('Ctrl Pts',(0.212629851289998,-0.0319640922340619,
-0.106518415216574));
#37255=CARTESIAN_POINT('Ctrl Pts',(0.142691686775344,0.160848389091954,
-0.0954405345467522));
#37256=CARTESIAN_POINT('Ctrl Pts',(-0.0570801517843907,0.207302254554576,
-0.0843626538769298));
#37257=CARTESIAN_POINT('Ctrl Pts',(-0.20491784206649,0.0651363028620932,
-0.0732847732071075));
#37258=CARTESIAN_POINT('Ctrl Pts',(-0.166294566507511,-0.136306265444277,
-0.0622068925372852));
#37259=CARTESIAN_POINT('Ctrl Pts',(0.0236289077939032,-0.213706425422127,
-0.0511290118674628));
#37260=CARTESIAN_POINT('Ctrl Pts',(0.19207415425848,-0.0966876067924717,
-0.0400511311976405));
#37261=CARTESIAN_POINT('Ctrl Pts',(0.185709484898353,0.108369764494427,
-0.0289732505278181));
#37262=CARTESIAN_POINT('Ctrl Pts',(0.0104465843032729,0.214702229009333,
-0.0178953698579959));
#37263=CARTESIAN_POINT('Ctrl Pts',(-0.174473318260629,0.125906390100295,
-0.00681748918817361));
#37264=CARTESIAN_POINT('Ctrl Pts',(-0.200341379572013,-0.07791109802852,
0.00426039148164884));
#37265=CARTESIAN_POINT('Ctrl Pts',(-0.0964954161413792,-0.165827445938701,
0.0116456452615303));
#37266=CARTESIAN_POINT('Ctrl Pts',(-0.0374209849651502,-0.178230609497964,
0.0153382721514711));
#37267=CARTESIAN_POINT('Ctrl Pts',(-0.0861525859670493,0.175382131162756,
-0.7746));
#37268=CARTESIAN_POINT('Ctrl Pts',(-0.144282890666663,0.146826906980443,
-0.77090737311006));
#37269=CARTESIAN_POINT('Ctrl Pts',(-0.228943378668034,0.0278940482341852,
-0.763522119330178));
#37270=CARTESIAN_POINT('Ctrl Pts',(-0.148019295174229,-0.177152683497377,
-0.752444238660355));
#37271=CARTESIAN_POINT('Ctrl Pts',(0.067776171560163,-0.220451388481608,
-0.741366357990533));
#37272=CARTESIAN_POINT('Ctrl Pts',(0.221805200709154,-0.0634399276354107,
-0.730288477320711));
#37273=CARTESIAN_POINT('Ctrl Pts',(0.174064020442395,0.151440409743154,
-0.719210596650888));
#37274=CARTESIAN_POINT('Ctrl Pts',(-0.0320847392583885,0.228449100319062,
-0.708132715981067));
#37275=CARTESIAN_POINT('Ctrl Pts',(-0.209025632592586,0.097631498265954,
-0.697054835311244));
#37276=CARTESIAN_POINT('Ctrl Pts',(-0.195781179656496,-0.122042005566363,
-0.685976954641422));
#37277=CARTESIAN_POINT('Ctrl Pts',(-0.00439137405617511,-0.230658383851736,
-0.674899073971599));
#37278=CARTESIAN_POINT('Ctrl Pts',(0.190992132722591,-0.129404198601949,
-0.663821193301777));
#37279=CARTESIAN_POINT('Ctrl Pts',(0.212592741982105,0.0895980348307404,
-0.652743312631955));
#37280=CARTESIAN_POINT('Ctrl Pts',(0.0407544219392627,0.227073328999068,
-0.641665431962132));
#37281=CARTESIAN_POINT('Ctrl Pts',(-0.168166100682019,0.157935180104365,
-0.630587551292311));
#37282=CARTESIAN_POINT('Ctrl Pts',(-0.224072253102051,-0.0549088034057021,
-0.619509670622487));
#37283=CARTESIAN_POINT('Ctrl Pts',(-0.0760947312113224,-0.217790975577677,
-0.608431789952666));
#37284=CARTESIAN_POINT('Ctrl Pts',(0.141121429607223,-0.182505015817326,
-0.597353909282842));
#37285=CARTESIAN_POINT('Ctrl Pts',(0.229931065789193,0.0188425254469469,
-0.586276028613023));
#37286=CARTESIAN_POINT('Ctrl Pts',(0.109526156171463,0.20304519848257,-0.575198147943197));
#37287=CARTESIAN_POINT('Ctrl Pts',(-0.110536719457191,0.202496835553871,
-0.564120267273377));
#37288=CARTESIAN_POINT('Ctrl Pts',(-0.230022113510055,0.0176963660989677,
-0.553042386603553));
#37289=CARTESIAN_POINT('Ctrl Pts',(-0.140210127285897,-0.183206041872212,
-0.541964505933732));
#37290=CARTESIAN_POINT('Ctrl Pts',(0.0771792098386744,-0.217409069767634,
-0.530886625263909));
#37291=CARTESIAN_POINT('Ctrl Pts',(0.224343097992066,-0.0537913403650071,
-0.519808744594087));
#37292=CARTESIAN_POINT('Ctrl Pts',(0.167376949885116,0.158771189159799,
-0.508730863924265));
#37293=CARTESIAN_POINT('Ctrl Pts',(-0.0418856721743048,0.226867636287773,
-0.497652983254443));
#37294=CARTESIAN_POINT('Ctrl Pts',(-0.213036474298089,0.0885369669856078,
-0.486575102584619));
#37295=CARTESIAN_POINT('Ctrl Pts',(-0.190345149926783,-0.130353587593923,
-0.475497221914798));
#37296=CARTESIAN_POINT('Ctrl Pts',(0.00554143943731765,-0.230635266942719,
-0.464419341244975));
#37297=CARTESIAN_POINT('Ctrl Pts',(0.196385866863427,-0.121061658674571,
-0.453341460575153));
#37298=CARTESIAN_POINT('Ctrl Pts',(0.208538574169865,0.0986660883364943,
-0.442263579905331));
#37299=CARTESIAN_POINT('Ctrl Pts',(0.0309417993812268,0.228617451120356,
-0.431185699235508));
#37300=CARTESIAN_POINT('Ctrl Pts',(-0.174808953305389,0.150549539186741,
-0.420107818565687));
#37301=CARTESIAN_POINT('Ctrl Pts',(-0.221500843678673,-0.0645035669922008,
-0.409029937895863));
#37302=CARTESIAN_POINT('Ctrl Pts',(-0.0666488684171745,-0.220864805353768,
-0.397952057226042));
#37303=CARTESIAN_POINT('Ctrl Pts',(0.148846986831278,-0.176260910063493,
-0.386874176556219));
#37304=CARTESIAN_POINT('Ctrl Pts',(0.228906802126409,0.028722984618816,
-0.375796295886397));
#37305=CARTESIAN_POINT('Ctrl Pts',(0.100684061903882,0.207571803440873,
-0.364718415216575));
#37306=CARTESIAN_POINT('Ctrl Pts',(-0.119151218961802,0.197550805933978,
-0.353640534546752));
#37307=CARTESIAN_POINT('Ctrl Pts',(-0.23057067230305,0.00777810894758914,
-0.34256265387693));
#37308=CARTESIAN_POINT('Ctrl Pts',(-0.132193612790705,-0.189071898076914,
-0.331484773207107));
#37309=CARTESIAN_POINT('Ctrl Pts',(0.0864665629929426,-0.213885173375585,
-0.320406892537285));
#37310=CARTESIAN_POINT('Ctrl Pts',(0.226450716306952,-0.0440840899701212,
-0.309329011867463));
#37311=CARTESIAN_POINT('Ctrl Pts',(0.16038710934437,0.1658291562449,-0.298251131197641));
#37312=CARTESIAN_POINT('Ctrl Pts',(-0.0516129079738391,0.224854267558481,
-0.287173250527818));
#37313=CARTESIAN_POINT('Ctrl Pts',(-0.216650282529325,0.0792842290699699,
-0.276095369857996));
#37314=CARTESIAN_POINT('Ctrl Pts',(-0.184557322500644,-0.138426618161985,
-0.265017489188174));
#37315=CARTESIAN_POINT('Ctrl Pts',(0.0154645519437773,-0.230182930647502,
-0.253939608518351));
#37316=CARTESIAN_POINT('Ctrl Pts',(0.20141521314946,-0.112495536675989,
-0.242861727848529));
#37317=CARTESIAN_POINT('Ctrl Pts',(0.204097946638625,0.107551671734282,
-0.231783847178707));
#37318=CARTESIAN_POINT('Ctrl Pts',(0.021071729584197,0.229737494242626,
-0.220705966508885));
#37319=CARTESIAN_POINT('Ctrl Pts',(-0.181127677032031,0.142884912377025,
-0.209628085839062));
#37320=CARTESIAN_POINT('Ctrl Pts',(-0.218518809022625,-0.0739788089933519,
-0.19855020516924));
#37321=CARTESIAN_POINT('Ctrl Pts',(-0.0570794292315143,-0.223529133484416,
-0.187472324499417));
#37322=CARTESIAN_POINT('Ctrl Pts',(0.156296581749669,-0.169690041092254,
-0.176394443829595));
#37323=CARTESIAN_POINT('Ctrl Pts',(0.22745816824746,0.0385501942625873,
-0.165316563159773));
#37324=CARTESIAN_POINT('Ctrl Pts',(0.0916552933376127,0.211713594027557,
-0.154238682489951));
#37325=CARTESIAN_POINT('Ctrl Pts',(-0.127544798487651,0.19223850171062,
-0.143160801820128));
#37326=CARTESIAN_POINT('Ctrl Pts',(-0.230691806051256,-0.00215451212232307,
-0.132082921150306));
#37327=CARTESIAN_POINT('Ctrl Pts',(-0.123931946417632,-0.194587335637062,
-0.121005040480483));
#37328=CARTESIAN_POINT('Ctrl Pts',(0.0955934736025586,-0.209964538565252,
-0.109927159810661));
#37329=CARTESIAN_POINT('Ctrl Pts',(0.228138773361758,-0.0342955081314312,
-0.0988492791408387));
#37330=CARTESIAN_POINT('Ctrl Pts',(0.153099417566957,0.172580444194569,
-0.0877713984710167));
#37331=CARTESIAN_POINT('Ctrl Pts',(-0.0612434977139372,0.222422589219168,
-0.0766935178011943));
#37332=CARTESIAN_POINT('Ctrl Pts',(-0.219864261040315,0.0698872531120333,
-0.065615637131372));
#37333=CARTESIAN_POINT('Ctrl Pts',(-0.178423858125201,-0.146248252591626,
-0.0545377564615497));
#37334=CARTESIAN_POINT('Ctrl Pts',(0.025352367070167,-0.229293871295783,
-0.0434598757917272));
#37335=CARTESIAN_POINT('Ctrl Pts',(0.20608377272137,-0.103739864741919,
-0.032381995121905));
#37336=CARTESIAN_POINT('Ctrl Pts',(0.199254873336532,0.116274102583752,
-0.0213041144520825));
#37337=CARTESIAN_POINT('Ctrl Pts',(0.0112085434585504,0.230362307395023,
-0.0102262337822604));
#37338=CARTESIAN_POINT('Ctrl Pts',(-0.187199156519412,0.135089824978115,
0.000851646887561937));
#37339=CARTESIAN_POINT('Ctrl Pts',(-0.214953997812966,-0.0835938238570844,
0.0119295275573844));
#37340=CARTESIAN_POINT('Ctrl Pts',(-0.103533655975248,-0.177922666439583,
0.0193147813372658));
#37341=CARTESIAN_POINT('Ctrl Pts',(-0.0401504189376249,-0.191230499291126,
0.0230074082272066));
#37342=CARTESIAN_POINT('',(-0.14957294282862,0.126218275177078,2.60208521396521E-16));
#37343=CARTESIAN_POINT('Ctrl Pts',(-0.149572942828615,0.126218275177084,
-1.90819582357449E-16));
#37344=CARTESIAN_POINT('Ctrl Pts',(-0.152409355584855,0.12213839882076,
-1.87889127479728E-16));
#37345=CARTESIAN_POINT('Ctrl Pts',(-0.155074825311664,0.117949841983875,
-2.1390244607528E-16));
#37346=CARTESIAN_POINT('Ctrl Pts',(-0.157558539584755,0.113656763614523,
-2.04697370165263E-16));
#37347=CARTESIAN_POINT('Ctrl Pts',(-0.162058150554841,0.105879225459084,
-1.88083489625304E-16));
#37348=CARTESIAN_POINT('Ctrl Pts',(-0.165961946681547,0.0977586786429782,
-1.12184872298018E-16));
#37349=CARTESIAN_POINT('Ctrl Pts',(-0.16926637762541,0.0893686620215524,
-8.32667268468867E-17));
#37350=CARTESIAN_POINT('Ctrl Pts',(-0.171514642330858,0.0836602727198771,
-6.35914342263728E-17));
#37351=CARTESIAN_POINT('Ctrl Pts',(-0.173486025552789,0.0778223415514922,
-5.15165993817366E-17));
#37352=CARTESIAN_POINT('Ctrl Pts',(-0.175169499051515,0.0719067612362681,
-5.55111512312578E-17));
#37353=CARTESIAN_POINT('Ctrl Pts',(-0.177114241837621,0.0650731032354923,
-6.01256437664607E-17));
#37354=CARTESIAN_POINT('Ctrl Pts',(-0.178678026440626,0.058129532159444,
-1.80244693759025E-17));
#37355=CARTESIAN_POINT('Ctrl Pts',(-0.179858327438416,0.0511127445516475,
-7.28583859910259E-17));
#37356=CARTESIAN_POINT('Ctrl Pts',(-0.18088836409873,0.0449892654669132,
-1.2071138657974E-16));
#37357=CARTESIAN_POINT('Ctrl Pts',(-0.181626262306867,0.0388099715919878,
1.20909457254854E-16));
#37358=CARTESIAN_POINT('Ctrl Pts',(-0.182067201079106,0.0325999030412639,
1.59594559789866E-16));
#37359=CARTESIAN_POINT('Ctrl Pts',(-0.182359376173048,0.028484983972151,
1.85228103898386E-16));
#37360=CARTESIAN_POINT('Ctrl Pts',(-0.182520385982331,0.0243657260406017,
2.37793219281459E-16));
#37361=CARTESIAN_POINT('Ctrl Pts',(-0.182550077425778,0.0202529927329005,
2.18575157973078E-16));
#37362=CARTESIAN_POINT('Ctrl Pts',(-0.182638158679569,0.00805234957811116,
1.61563752027702E-16));
#37363=CARTESIAN_POINT('Ctrl Pts',(-0.181574880217677,-0.00410296492725809,
-4.2435135068192E-18));
#37364=CARTESIAN_POINT('Ctrl Pts',(-0.17933098841831,-0.01602004498147,
-3.29597460435593E-17));
#37365=CARTESIAN_POINT('Ctrl Pts',(-0.178221946841473,-0.0219100514685647,
-4.71527190836742E-17));
#37366=CARTESIAN_POINT('Ctrl Pts',(-0.176823766898375,-0.0277415985898121,
-1.23108892831518E-16));
#37367=CARTESIAN_POINT('Ctrl Pts',(-0.175128724846193,-0.0334888034719142,
-1.196959198424E-16));
#37368=CARTESIAN_POINT('Ctrl Pts',(-0.174065414734053,-0.0370940597897774,
-1.17554941282537E-16));
#37369=CARTESIAN_POINT('Ctrl Pts',(-0.172884634981322,-0.0406668331426877,
4.85499834843578E-16));
#37370=CARTESIAN_POINT('Ctrl Pts',(-0.171590404833548,-0.0441852584481628,
4.28476698566271E-16));
#37371=CARTESIAN_POINT('Ctrl Pts',(-0.169183900073534,-0.050727454409171,
3.22447296362707E-16));
#37372=CARTESIAN_POINT('Ctrl Pts',(-0.166382027562676,-0.0570950810552904,
-3.16274383796401E-17));
#37373=CARTESIAN_POINT('Ctrl Pts',(-0.163177510429029,-0.0632495561099533,
-3.46944695195361E-18));
#37374=CARTESIAN_POINT('Ctrl Pts',(-0.159378089464225,-0.0705465810827711,
2.98008237155791E-17));
#37375=CARTESIAN_POINT('Ctrl Pts',(-0.155012614776842,-0.0775443065037668,
1.01748044056608E-16));
#37376=CARTESIAN_POINT('Ctrl Pts',(-0.150134094058049,-0.0842019941615851,
1.47451495458029E-16));
#37377=CARTESIAN_POINT('Ctrl Pts',(-0.147447444266624,-0.0878684488490376,
1.72620839866475E-16));
#37378=CARTESIAN_POINT('Ctrl Pts',(-0.144605056887674,-0.0914316066797669,
4.6437475298905E-17));
#37379=CARTESIAN_POINT('Ctrl Pts',(-0.141615068278682,-0.094883245817762,
-1.21430643318376E-17));
#37380=CARTESIAN_POINT('Ctrl Pts',(-0.139243928227529,-0.0976204869489193,
-5.85989816951453E-17));
#37381=CARTESIAN_POINT('Ctrl Pts',(-0.136785305582189,-0.100281264847667,
-5.84262065888997E-17));
#37382=CARTESIAN_POINT('Ctrl Pts',(-0.134247412155013,-0.102859257524588,
-4.5102810375397E-17));
#37383=CARTESIAN_POINT('Ctrl Pts',(-0.127464722402785,-0.109749115200969,
-9.49514379865841E-18));
#37384=CARTESIAN_POINT('Ctrl Pts',(-0.120109608121736,-0.116057478078322,
-2.73862375609035E-17));
#37385=CARTESIAN_POINT('Ctrl Pts',(-0.112270412127471,-0.121716646311139,
6.07153216591882E-18));
#37386=CARTESIAN_POINT('Ctrl Pts',(-0.107173860027412,-0.125395881498351,
2.78236693352516E-17));
#37387=CARTESIAN_POINT('Ctrl Pts',(-0.101872390808594,-0.128800281258816,
1.78627078510015E-16));
#37388=CARTESIAN_POINT('Ctrl Pts',(-0.0963888361066501,-0.131905437921845,
1.97758476261356E-16));
#37389=CARTESIAN_POINT('Ctrl Pts',(-0.092445112883218,-0.134138638666618,
2.11517605459416E-16));
#37390=CARTESIAN_POINT('Ctrl Pts',(-0.0884032420310201,-0.13621834887122,
-2.35626616501682E-16));
#37391=CARTESIAN_POINT('Ctrl Pts',(-0.0842970527965122,-0.138123431873126,
-2.03396327558281E-16));
#37392=CARTESIAN_POINT('Ctrl Pts',(-0.0745227262503713,-0.142658269966226,
-1.26675711235531E-16));
#37393=CARTESIAN_POINT('Ctrl Pts',(-0.0643598268954344,-0.146223024533765,
-1.39475126112393E-16));
#37394=CARTESIAN_POINT('Ctrl Pts',(-0.0539300424733775,-0.148702066835777,
-1.03432887255117E-16));
#37395=CARTESIAN_POINT('Ctrl Pts',(-0.0467211978956824,-0.150415528009428,
-7.85212603565983E-17));
#37396=CARTESIAN_POINT('Ctrl Pts',(-0.039384578838078,-0.151609390787265,
-5.55933009525148E-18));
#37397=CARTESIAN_POINT('Ctrl Pts',(-0.0319621170202007,-0.152230829911641,
-1.73472347597681E-18));
#37398=CARTESIAN_POINT('Ctrl Pts',(-0.195258838497135,0.000160033407109407,
-0.0621869692124234));
#37399=CARTESIAN_POINT('Ctrl Pts',(-0.194908302996182,-0.0446298405868324,
-0.0596372316287988));
#37400=CARTESIAN_POINT('Ctrl Pts',(-0.179587999130102,-0.0896361310987459,
-0.0570874940451742));
#37401=CARTESIAN_POINT('Ctrl Pts',(-0.151367887745159,-0.124066604758376,
-0.0545377564615496));
#37402=CARTESIAN_POINT('Ctrl Pts',(-0.110498449726745,-0.173930125493011,
-0.0508451295716089));
#37403=CARTESIAN_POINT('Ctrl Pts',(-0.0425730413282883,-0.201611998394397,
-0.047152502681668));
#37404=CARTESIAN_POINT('Ctrl Pts',(0.0215115638128062,-0.194527267086113,
-0.0434598757917273));
#37405=CARTESIAN_POINT('Ctrl Pts',(0.0855961689539017,-0.187442535777828,
-0.0397672489017865));
#37406=CARTESIAN_POINT('Ctrl Pts',(0.145839970837636,-0.145591200259874,
-0.0360746220118458));
#37407=CARTESIAN_POINT('Ctrl Pts',(0.17482372188203,-0.0879965379466177,
-0.032381995121905));
#37408=CARTESIAN_POINT('Ctrl Pts',(0.203807472926425,-0.0304018756333616,
-0.0286893682319642));
#37409=CARTESIAN_POINT('Ctrl Pts',(0.201531173131478,0.0429361134751947,
-0.0249967413420234));
#37410=CARTESIAN_POINT('Ctrl Pts',(0.169051968254342,0.0986198088313519,
-0.0213041144520826));
#37411=CARTESIAN_POINT('Ctrl Pts',(0.136572763377205,0.154303504187508,
-0.0176114875621418));
#37412=CARTESIAN_POINT('Ctrl Pts',(0.0738906534178767,0.192332905791266,
-0.013918860672201));
#37413=CARTESIAN_POINT('Ctrl Pts',(0.00948164844188619,0.19546885952366,
-0.0102262337822603));
#37414=CARTESIAN_POINT('Ctrl Pts',(-0.0499757118780851,0.198363726958473,
-0.00681748918817344));
#37415=CARTESIAN_POINT('Ctrl Pts',(-0.110904652631899,0.171524004472446,
-0.00340874459408663));
#37416=CARTESIAN_POINT('Ctrl Pts',(-0.14957294282862,0.126218275177078,
2.60208521396521E-16));
#37417=CARTESIAN_POINT('',(-0.0903606778650212,-0.126612599672283,-0.7746));
#37418=CARTESIAN_POINT('Ctrl Pts',(-0.0905528965052105,-0.126780367713603,
-0.7746));
#37419=CARTESIAN_POINT('Ctrl Pts',(-0.0940851012826834,-0.124893446464691,
-0.7746));
#37420=CARTESIAN_POINT('Ctrl Pts',(-0.0975325099084221,-0.122865237059866,
-0.7746));
#37421=CARTESIAN_POINT('Ctrl Pts',(-0.100885595415379,-0.120697716718052,
-0.7746));
#37422=CARTESIAN_POINT('Ctrl Pts',(-0.108471912208483,-0.115793727262852,
-0.7746));
#37423=CARTESIAN_POINT('Ctrl Pts',(-0.115576183595968,-0.11017842588183,
-0.7746));
#37424=CARTESIAN_POINT('Ctrl Pts',(-0.122169299632121,-0.103959921816958,
-0.7746));
#37425=CARTESIAN_POINT('Ctrl Pts',(-0.124862496418268,-0.101419748844069,
-0.7746));
#37426=CARTESIAN_POINT('Ctrl Pts',(-0.127468591019258,-0.0987799359225111,
-0.7746));
#37427=CARTESIAN_POINT('Ctrl Pts',(-0.129979488448584,-0.0960543571919703,
-0.7746));
#37428=CARTESIAN_POINT('Ctrl Pts',(-0.135808916607278,-0.0897265139216807,
-0.7746));
#37429=CARTESIAN_POINT('Ctrl Pts',(-0.141135846833842,-0.0829282927568507,
-0.7746));
#37430=CARTESIAN_POINT('Ctrl Pts',(-0.145934371304684,-0.0757454531871112,
-0.7746));
#37431=CARTESIAN_POINT('Ctrl Pts',(-0.149045007814598,-0.0710891878817545,
-0.7746));
#37432=CARTESIAN_POINT('Ctrl Pts',(-0.151935890614529,-0.0662652353489526,
-0.7746));
#37433=CARTESIAN_POINT('Ctrl Pts',(-0.154582417168357,-0.0613252527221335,
-0.7746));
#37434=CARTESIAN_POINT('Ctrl Pts',(-0.160106278576474,-0.0510144627738566,
-0.7746));
#37435=CARTESIAN_POINT('Ctrl Pts',(-0.164582453970299,-0.0401834658705794,
-0.7746));
#37436=CARTESIAN_POINT('Ctrl Pts',(-0.167945042441492,-0.0290261639881964,
-0.7746));
#37437=CARTESIAN_POINT('Ctrl Pts',(-0.169541196767554,-0.0237300131748207,
-0.7746));
#37438=CARTESIAN_POINT('Ctrl Pts',(-0.170885936193958,-0.0183597450823107,
-0.7746));
#37439=CARTESIAN_POINT('Ctrl Pts',(-0.171968925586268,-0.0129337153015973,
-0.7746));
#37440=CARTESIAN_POINT('Ctrl Pts',(-0.172843537099442,-0.00855170736067374,
-0.7746));
#37441=CARTESIAN_POINT('Ctrl Pts',(-0.173547366331531,-0.0041299597130302,
-0.7746));
#37442=CARTESIAN_POINT('Ctrl Pts',(-0.174071922613245,0.000296384781912512,
-0.7746));
#37443=CARTESIAN_POINT('Ctrl Pts',(-0.17489447630929,0.00723731019107897,
-0.7746));
#37444=CARTESIAN_POINT('Ctrl Pts',(-0.175279511390988,0.0142012653081574,
-0.7746));
#37445=CARTESIAN_POINT('Ctrl Pts',(-0.175212365254669,0.0211498412838069,
-0.7746));
#37446=CARTESIAN_POINT('Ctrl Pts',(-0.175138215020913,0.0288232319077874,
-0.7746));
#37447=CARTESIAN_POINT('Ctrl Pts',(-0.174512946184563,0.0364780095010279,
-0.7746));
#37448=CARTESIAN_POINT('Ctrl Pts',(-0.173371562479243,0.0440753847157037,
-0.7746));
#37449=CARTESIAN_POINT('Ctrl Pts',(-0.172636569880567,0.0489677049110253,
-0.7746));
#37450=CARTESIAN_POINT('Ctrl Pts',(-0.171687349129919,0.0538362733301391,
-0.7746));
#37451=CARTESIAN_POINT('Ctrl Pts',(-0.170531114314323,0.0586708415584075,
-0.7746));
#37452=CARTESIAN_POINT('Ctrl Pts',(-0.169750782077226,0.0619336471668159,
-0.7746));
#37453=CARTESIAN_POINT('Ctrl Pts',(-0.168876703665589,0.0651778442623389,
-0.7746));
#37454=CARTESIAN_POINT('Ctrl Pts',(-0.167914250210792,0.0683919284573595,
-0.7746));
#37455=CARTESIAN_POINT('Ctrl Pts',(-0.164635838743272,0.0793400843707924,
-0.7746));
#37456=CARTESIAN_POINT('Ctrl Pts',(-0.160328586154646,0.0899671574594893,
-0.7746));
#37457=CARTESIAN_POINT('Ctrl Pts',(-0.155100469158035,0.100152140039335,
-0.7746));
#37458=CARTESIAN_POINT('Ctrl Pts',(-0.151778955638379,0.106622836345163,
-0.7746));
#37459=CARTESIAN_POINT('Ctrl Pts',(-0.148084885651745,0.112915234045713,
-0.7746));
#37460=CARTESIAN_POINT('Ctrl Pts',(-0.144037924095902,0.118997135380321,
-0.7746));
#37461=CARTESIAN_POINT('Ctrl Pts',(-0.141313178735255,0.123091968557436,
-0.7746));
#37462=CARTESIAN_POINT('Ctrl Pts',(-0.138425284714667,0.127094620860079,
-0.7746));
#37463=CARTESIAN_POINT('Ctrl Pts',(-0.135397693361022,0.130972343961411,
-0.7746));
#37464=CARTESIAN_POINT('Ctrl Pts',(-0.127505121547234,0.141081108479578,
-0.7746));
#37465=CARTESIAN_POINT('Ctrl Pts',(-0.118649514256097,0.150371904390044,
-0.7746));
#37466=CARTESIAN_POINT('Ctrl Pts',(-0.108949064714297,0.158681874715884,
-0.7746));
#37467=CARTESIAN_POINT('Ctrl Pts',(-0.101799585751722,0.164806534997679,
-0.7746));
#37468=CARTESIAN_POINT('Ctrl Pts',(-0.0941900010005582,0.170398440943833,
-0.7746));
#37469=CARTESIAN_POINT('Ctrl Pts',(-0.0861525859670496,0.175382131162756,
-0.7746));
#37470=CARTESIAN_POINT('Ctrl Pts',(-0.0905528965052109,-0.126780367713602,
-0.7746));
#37471=CARTESIAN_POINT('Ctrl Pts',(-0.0518141871612445,-0.154123000442621,
-0.771191255405913));
#37472=CARTESIAN_POINT('Ctrl Pts',(0.0570960259948757,-0.17228938136959,
-0.764089883921885));
#37473=CARTESIAN_POINT('Ctrl Pts',(0.176570107319903,-0.0505019485347378,
-0.753295885547919));
#37474=CARTESIAN_POINT('Ctrl Pts',(0.138565293653093,0.120555556476704,
-0.742218004878094));
#37475=CARTESIAN_POINT('Ctrl Pts',(-0.0255413571731973,0.181859045827175,
-0.731140124208274));
#37476=CARTESIAN_POINT('Ctrl Pts',(-0.140076662830731,0.0971797286032077,
-0.722132248395451));
#37477=CARTESIAN_POINT('Ctrl Pts',(-0.155378700824008,0.0227870178177375,
-0.71681699947257));
#37478=CARTESIAN_POINT('Ctrl Pts',(-0.155313284670072,5.07842058496948E-5,
-0.71519437743963));
#37479=CARTESIAN_POINT('Origin',(-2.59090492670967E-17,0.,-0.7746));
#37480=CARTESIAN_POINT('',(-0.1954,-2.39295984553393E-17,-0.7746));
#37481=CARTESIAN_POINT('Origin',(0.,0.,-0.7746));
#37482=CARTESIAN_POINT('Origin',(0.,0.,-0.7746));
#37483=CARTESIAN_POINT('',(0.0903606778650188,-0.126612599672285,-0.7746));
#37484=CARTESIAN_POINT('Ctrl Pts',(0.0863566189666514,0.175629287040325,
-0.7746));
#37485=CARTESIAN_POINT('Ctrl Pts',(0.0905917700201877,0.173030418616691,
-0.7746));
#37486=CARTESIAN_POINT('Ctrl Pts',(0.0947139527180262,0.17026341030673,
-0.7746));
#37487=CARTESIAN_POINT('Ctrl Pts',(0.0987115944104381,0.167327732998805,
-0.7746));
#37488=CARTESIAN_POINT('Ctrl Pts',(0.105953907859282,0.162009323575319,
-0.7746));
#37489=CARTESIAN_POINT('Ctrl Pts',(0.112788112244188,0.156137654118489,
-0.7746));
#37490=CARTESIAN_POINT('Ctrl Pts',(0.119181447487494,0.149778658377445,
-0.7746));
#37491=CARTESIAN_POINT('Ctrl Pts',(0.123531334816534,0.145452134904685,
-0.7746));
#37492=CARTESIAN_POINT('Ctrl Pts',(0.127679589020936,0.14089585436879,-0.7746));
#37493=CARTESIAN_POINT('Ctrl Pts',(0.131595286168026,0.136152923130775,
-0.7746));
#37494=CARTESIAN_POINT('Ctrl Pts',(0.136118691747208,0.130673898370227,
-0.7746));
#37495=CARTESIAN_POINT('Ctrl Pts',(0.14033725682518,0.124941332985309,-0.7746));
#37496=CARTESIAN_POINT('Ctrl Pts',(0.14423394336631,0.118987826111841,-0.7746));
#37497=CARTESIAN_POINT('Ctrl Pts',(0.147634565650473,0.113792225200879,
-0.7746));
#37498=CARTESIAN_POINT('Ctrl Pts',(0.150789992297107,0.108428273261232,
-0.7746));
#37499=CARTESIAN_POINT('Ctrl Pts',(0.153685759550622,0.102916971941204,
-0.7746));
#37500=CARTESIAN_POINT('Ctrl Pts',(0.155604519974895,0.0992651360257737,
-0.7746));
#37501=CARTESIAN_POINT('Ctrl Pts',(0.157404880950174,0.0955566958497009,
-0.7746));
#37502=CARTESIAN_POINT('Ctrl Pts',(0.159082343688173,0.0918015394804238,
-0.7746));
#37503=CARTESIAN_POINT('Ctrl Pts',(0.16405867800029,0.0806615522458402,
-0.7746));
#37504=CARTESIAN_POINT('Ctrl Pts',(0.167962220294764,0.06910108595545,-0.7746));
#37505=CARTESIAN_POINT('Ctrl Pts',(0.170688770138284,0.0572850954713528,
-0.7746));
#37506=CARTESIAN_POINT('Ctrl Pts',(0.172036365341412,0.0514450510891004,
-0.7746));
#37507=CARTESIAN_POINT('Ctrl Pts',(0.173095662873938,0.0455425323535238,
-0.7746));
#37508=CARTESIAN_POINT('Ctrl Pts',(0.173849202315553,0.0395981476128783,
-0.7746));
#37509=CARTESIAN_POINT('Ctrl Pts',(0.174321899067488,0.0358692235460382,
-0.7746));
#37510=CARTESIAN_POINT('Ctrl Pts',(0.174673965346606,0.0321229165232209,
-0.7746));
#37511=CARTESIAN_POINT('Ctrl Pts',(0.174900309122346,0.028380866512874,
-0.7746));
#37512=CARTESIAN_POINT('Ctrl Pts',(0.175321177537221,0.0214228193958648,
-0.7746));
#37513=CARTESIAN_POINT('Ctrl Pts',(0.175309856312594,0.0144660238244896,
-0.7746));
#37514=CARTESIAN_POINT('Ctrl Pts',(0.174844198658199,0.00754289949041315,
-0.7746));
#37515=CARTESIAN_POINT('Ctrl Pts',(0.174292106830062,-0.000665277340672647,
-0.7746));
#37516=CARTESIAN_POINT('Ctrl Pts',(0.173101464382142,-0.00882644735382486,
-0.7746));
#37517=CARTESIAN_POINT('Ctrl Pts',(0.171304475172341,-0.016882029516175,
-0.7746));
#37518=CARTESIAN_POINT('Ctrl Pts',(0.170314958987332,-0.0213178541086821,
-0.7746));
#37519=CARTESIAN_POINT('Ctrl Pts',(0.169141391072696,-0.0257215634108893,
-0.7746));
#37520=CARTESIAN_POINT('Ctrl Pts',(0.167787923338702,-0.0300823658649688,
-0.7746));
#37521=CARTESIAN_POINT('Ctrl Pts',(0.166714256292423,-0.0335416650951491,
-0.7746));
#37522=CARTESIAN_POINT('Ctrl Pts',(0.165529733571263,-0.0369660268452503,
-0.7746));
#37523=CARTESIAN_POINT('Ctrl Pts',(0.164239345981684,-0.040346349804367,
-0.7746));
#37524=CARTESIAN_POINT('Ctrl Pts',(0.16079130903207,-0.0493788905376982,
-0.7746));
#37525=CARTESIAN_POINT('Ctrl Pts',(0.156585614990708,-0.0581084965167856,
-0.774600000000001));
#37526=CARTESIAN_POINT('Ctrl Pts',(0.151676017384677,-0.0664377067708377,
-0.774600000000001));
#37527=CARTESIAN_POINT('Ctrl Pts',(0.148484180335376,-0.0718527089794996,
-0.774600000000001));
#37528=CARTESIAN_POINT('Ctrl Pts',(0.144994377343054,-0.0770982050079457,
-0.7746));
#37529=CARTESIAN_POINT('Ctrl Pts',(0.141217726682289,-0.0821426785805183,
-0.7746));
#37530=CARTESIAN_POINT('Ctrl Pts',(0.138501407060657,-0.0857708676233492,
-0.7746));
#37531=CARTESIAN_POINT('Ctrl Pts',(0.135633582499286,-0.0892978390970129,
-0.7746));
#37532=CARTESIAN_POINT('Ctrl Pts',(0.132636760309005,-0.0926906541131664,
-0.7746));
#37533=CARTESIAN_POINT('Ctrl Pts',(0.125503512371863,-0.100766472155882,
-0.7746));
#37534=CARTESIAN_POINT('Ctrl Pts',(0.117625088446425,-0.108109649572534,
-0.7746));
#37535=CARTESIAN_POINT('Ctrl Pts',(0.109066551488383,-0.114565445008817,
-0.7746));
#37536=CARTESIAN_POINT('Ctrl Pts',(0.103151057383426,-0.119027565115719,
-0.7746));
#37537=CARTESIAN_POINT('Ctrl Pts',(0.0969100292154159,-0.123065020826135,
-0.7746));
#37538=CARTESIAN_POINT('Ctrl Pts',(0.0903606778650199,-0.126612599672284,
-0.7746));
#37539=CARTESIAN_POINT('Origin',(0.,0.,-0.7746));
#37540=CARTESIAN_POINT('Origin',(0.,0.,-0.90400562256037));
#37541=CARTESIAN_POINT('Ctrl Pts',(0.0903606778650188,-0.126612599672285,
-0.7746));
#37542=CARTESIAN_POINT('Ctrl Pts',(0.132326349903352,-0.0966626058939412,
-0.77090737311006));
#37543=CARTESIAN_POINT('Ctrl Pts',(0.183438243169013,0.00770935888928891,
-0.763522119330179));
#37544=CARTESIAN_POINT('Ctrl Pts',(0.0933467737565466,0.158298955986194,
-0.752444238660355));
#37545=CARTESIAN_POINT('Ctrl Pts',(-0.0817572628182647,0.164390938130267,
-0.741366357990534));
#37546=CARTESIAN_POINT('Ctrl Pts',(-0.152758625409659,0.0633569399596061,
-0.733553485957205));
#37547=CARTESIAN_POINT('Ctrl Pts',(-0.155762614151669,0.00605970375071522,
-0.729433240813817));
#37548=CARTESIAN_POINT('Ctrl Pts',(-0.155718793124499,0.000108222005882058,
-0.72900562256037));
#37549=CARTESIAN_POINT('Ctrl Pts',(0.113509973994371,-0.159049193030953,
-0.797607408227207));
#37550=CARTESIAN_POINT('Ctrl Pts',(0.166226735912021,-0.12142637860287,
-0.793914781337266));
#37551=CARTESIAN_POINT('Ctrl Pts',(0.230432868628899,0.0096844019734276,
-0.786529527557385));
#37552=CARTESIAN_POINT('Ctrl Pts',(0.117261070987011,0.198853204755397,
-0.775451646887562));
#37553=CARTESIAN_POINT('Ctrl Pts',(-0.102702469654057,0.206505877921275,
-0.76437376621774));
#37554=CARTESIAN_POINT('Ctrl Pts',(-0.229166552539487,0.026549163675777,
-0.753295885547918));
#37555=CARTESIAN_POINT('Ctrl Pts',(-0.147138184514376,-0.177715596359759,
-0.742218004878095));
#37556=CARTESIAN_POINT('Ctrl Pts',(0.0687852681232544,-0.220197695999892,
-0.731140124208273));
#37557=CARTESIAN_POINT('Ctrl Pts',(0.222113639748162,-0.0623631311604367,
-0.720062243538451));
#37558=CARTESIAN_POINT('Ctrl Pts',(0.173344387514496,0.152237478465231,
-0.708984362868628));
#37559=CARTESIAN_POINT('Ctrl Pts',(-0.0331531249511722,0.228305613963639,
-0.697906482198806));
#37560=CARTESIAN_POINT('Ctrl Pts',(-0.20948351797168,0.0966442108510496,
-0.686828601528984));
#37561=CARTESIAN_POINT('Ctrl Pts',(-0.195205176657611,-0.122957014602741,
-0.675750720859161));
#37562=CARTESIAN_POINT('Ctrl Pts',(-0.0033091362147546,-0.230677863194179,
-0.664672840189339));
#37563=CARTESIAN_POINT('Ctrl Pts',(0.191597738574492,-0.128505532717413,
-0.653594959519517));
#37564=CARTESIAN_POINT('Ctrl Pts',(0.212169696530742,0.0905945808558615,
-0.642517078849694));
#37565=CARTESIAN_POINT('Ctrl Pts',(0.0396881681025756,0.22726234506108,
-0.631439198179872));
#37566=CARTESIAN_POINT('Ctrl Pts',(-0.168905646876196,0.15714397242725,
-0.62036131751005));
#37567=CARTESIAN_POINT('Ctrl Pts',(-0.223812036237873,-0.055959942437397,
-0.609283436840227));
#37568=CARTESIAN_POINT('Ctrl Pts',(-0.0750715971962314,-0.218145808496258,
-0.598205556170405));
#37569=CARTESIAN_POINT('Ctrl Pts',(0.141976568990925,-0.181840577314685,
-0.587127675500583));
#37570=CARTESIAN_POINT('Ctrl Pts',(0.229840097781903,0.0199216082515445,
-0.576049794830761));
#37571=CARTESIAN_POINT('Ctrl Pts',(0.10857186341542,0.203557095173597,-0.564971914160938));
#37572=CARTESIAN_POINT('Ctrl Pts',(-0.111486030559036,0.201975755934477,
-0.553894033491116));
#37573=CARTESIAN_POINT('Ctrl Pts',(-0.230102660760181,0.0166164488813726,
-0.542816152821293));
#37574=CARTESIAN_POINT('Ctrl Pts',(-0.139348622206933,-0.183862182889048,
-0.531738272151472));
#37575=CARTESIAN_POINT('Ctrl Pts',(0.0781988836276648,-0.217044408992555,
-0.520660391481649));
#37576=CARTESIAN_POINT('Ctrl Pts',(0.22459313774015,-0.0527376841718607,
-0.509582510811826));
#37577=CARTESIAN_POINT('Ctrl Pts',(0.166629844370711,0.159555118412653,
-0.498504630142004));
#37578=CARTESIAN_POINT('Ctrl Pts',(-0.0429501309254399,0.226668540185073,
-0.487426749472182));
#37579=CARTESIAN_POINT('Ctrl Pts',(-0.213449734014577,0.0875360034570956,
-0.476348868802359));
#37580=CARTESIAN_POINT('Ctrl Pts',(-0.18973118516252,-0.131245640798648,
-0.465270988132538));
#37581=CARTESIAN_POINT('Ctrl Pts',(0.00662398147309128,-0.230606729569085,
-0.454193107462714));
#37582=CARTESIAN_POINT('Ctrl Pts',(0.196951979951472,-0.120138496934387,
-0.443115226792893));
#37583=CARTESIAN_POINT('Ctrl Pts',(0.208073151382307,0.0996438885547388,
-0.43203734612307));
#37584=CARTESIAN_POINT('Ctrl Pts',(0.0298683294310498,0.22876018829691,
-0.420959465453248));
#37585=CARTESIAN_POINT('Ctrl Pts',(-0.175513718907489,0.149727336608304,
-0.409881584783426));
#37586=CARTESIAN_POINT('Ctrl Pts',(-0.221195637922984,-0.0655425862808919,
-0.398803704113603));
#37587=CARTESIAN_POINT('Ctrl Pts',(-0.0656113983622211,-0.2211752365377,
-0.387725823443782));
#37588=CARTESIAN_POINT('Ctrl Pts',(0.149672726021042,-0.175560291461564,
-0.376647942773958));
#37589=CARTESIAN_POINT('Ctrl Pts',(0.228769469437527,0.0297971593569934,
-0.365570062104137));
#37590=CARTESIAN_POINT('Ctrl Pts',(0.0997086165043611,0.208042141517638,
-0.354492181434313));
#37591=CARTESIAN_POINT('Ctrl Pts',(-0.120077218212226,0.19698934620816,
-0.343414300764492));
#37592=CARTESIAN_POINT('Ctrl Pts',(-0.230604657647227,0.0066957242496528,
-0.33233642009467));
#37593=CARTESIAN_POINT('Ctrl Pts',(-0.131304660930752,-0.189690344693647,
-0.321258539424847));
#37594=CARTESIAN_POINT('Ctrl Pts',(0.0874695937736782,-0.21347695665156,
-0.310180658755026));
#37595=CARTESIAN_POINT('Ctrl Pts',(0.22665516716062,-0.0430206467417004,
-0.299102778085202));
#37596=CARTESIAN_POINT('Ctrl Pts',(0.159606950243788,0.16658019775968,-0.288024897415381));
#37597=CARTESIAN_POINT('Ctrl Pts',(-0.0526678094533962,0.22460953390923,
-0.276947016745558));
#37598=CARTESIAN_POINT('Ctrl Pts',(-0.217020070229199,0.0782664035548432,
-0.265869136075736));
#37599=CARTESIAN_POINT('Ctrl Pts',(-0.183905526410112,-0.139291414732429,
-0.254791255405913));
#37600=CARTESIAN_POINT('Ctrl Pts',(0.0165448622730762,-0.230107819353187,
-0.243713374736092));
#37601=CARTESIAN_POINT('Ctrl Pts',(0.201941061299588,-0.111548860515046,
-0.232635494066268));
#37602=CARTESIAN_POINT('Ctrl Pts',(0.20359086438931,0.10850852943864,-0.221557613396447));
#37603=CARTESIAN_POINT('Ctrl Pts',(0.0199931085929222,0.229833890689264,
-0.210479732726624));
#37604=CARTESIAN_POINT('Ctrl Pts',(-0.181796392508897,0.142033130433819,
-0.199401852056802));
#37605=CARTESIAN_POINT('Ctrl Pts',(-0.218169165091539,-0.0750037207463776,
-0.188323971386979));
#37606=CARTESIAN_POINT('Ctrl Pts',(-0.0560295462102443,-0.223794628104333,
-0.177246090717157));
#37607=CARTESIAN_POINT('Ctrl Pts',(0.157091373949139,-0.168954503937514,
-0.166168210047335));
#37608=CARTESIAN_POINT('Ctrl Pts',(0.22727476385837,0.0396174193949855,
-0.155090329377513));
#37609=CARTESIAN_POINT('Ctrl Pts',(0.0906604263794466,0.212141585867888,
-0.14401244870769));
#37610=CARTESIAN_POINT('Ctrl Pts',(-0.128445619592358,0.191637547881033,
-0.132934568037868));
#37611=CARTESIAN_POINT('Ctrl Pts',(-0.230679452575857,-0.00323706553079172,
-0.121856687368046));
#37612=CARTESIAN_POINT('Ctrl Pts',(-0.123016650143841,-0.195167496218507,
-0.110778806698223));
#37613=CARTESIAN_POINT('Ctrl Pts',(0.096576961801934,-0.209512466241152,
-0.0997009260284009));
#37614=CARTESIAN_POINT('Ctrl Pts',(0.228299237964294,-0.0332262618594141,
-0.0886230453585787));
#37615=CARTESIAN_POINT('Ctrl Pts',(0.152283875490699,0.173301039684831,
-0.0775451646887562));
#37616=CARTESIAN_POINT('Ctrl Pts',(-0.0622796920736053,0.222125366380487,
-0.066467284018934));
#37617=CARTESIAN_POINT('Ctrl Pts',(-0.220203600073336,0.0688683747915814,
-0.0553894033491115));
#37618=CARTESIAN_POINT('Ctrl Pts',(-0.177709301322904,-0.147110744400408,
-0.0443115226792893));
#37619=CARTESIAN_POINT('Ctrl Pts',(0.0263784818207279,-0.229121475610455,
-0.0332336420094669));
#37620=CARTESIAN_POINT('Ctrl Pts',(0.206664974128708,-0.102870521914166,
-0.0221557613396446));
#37621=CARTESIAN_POINT('Ctrl Pts',(0.198510833186043,0.117416113433844,
-0.0110778806698224));
#37622=CARTESIAN_POINT('Ctrl Pts',(0.0732416199231106,0.192383362751592,
-0.00369262688994078));
#37623=CARTESIAN_POINT('Ctrl Pts',(0.00853826423430079,0.19521336543348,
0.));
#37624=CARTESIAN_POINT('Ctrl Pts',(0.105793541951254,-0.14823699524473,
-0.789938272151471));
#37625=CARTESIAN_POINT('Ctrl Pts',(0.154926607242464,-0.113171787699894,
-0.786245645261531));
#37626=CARTESIAN_POINT('Ctrl Pts',(0.214767993475604,0.00902605427871468,
-0.778860391481649));
#37627=CARTESIAN_POINT('Ctrl Pts',(0.109289638576856,0.185335121832329,
-0.767782510811827));
#37628=CARTESIAN_POINT('Ctrl Pts',(-0.0957207340421262,0.192467564657606,
-0.756704630142005));
#37629=CARTESIAN_POINT('Ctrl Pts',(-0.213587761821816,0.0247443459131021,
-0.745626749472182));
#37630=CARTESIAN_POINT('Ctrl Pts',(-0.137135699606669,-0.165634452526706,
-0.73454886880236));
#37631=CARTESIAN_POINT('Ctrl Pts',(0.0641092310459577,-0.205228610046981,
-0.723470988132537));
#37632=CARTESIAN_POINT('Ctrl Pts',(0.207014307533962,-0.0581236723123581,
-0.712393107462715));
#37633=CARTESIAN_POINT('Ctrl Pts',(0.161560399383393,0.141888342476082,
-0.701315226792893));
#37634=CARTESIAN_POINT('Ctrl Pts',(-0.0308993685040486,0.21278535003247,
-0.69023734612307));
#37635=CARTESIAN_POINT('Ctrl Pts',(-0.195242784107519,0.0900743169540612,
-0.679159465453249));
#37636=CARTESIAN_POINT('Ctrl Pts',(-0.181935087456304,-0.114598370740716,
-0.668081584783425));
#37637=CARTESIAN_POINT('Ctrl Pts',(-0.00308418043488711,-0.214996333258512,
-0.657003704113604));
#37638=CARTESIAN_POINT('Ctrl Pts',(0.178572883777165,-0.119769699420263,
-0.645925823443782));
#37639=CARTESIAN_POINT('Ctrl Pts',(0.197746355679923,0.0844359420856367,
-0.634847942773959));
#37640=CARTESIAN_POINT('Ctrl Pts',(0.0369901580396483,0.211813002770593,
-0.623770062104137));
#37641=CARTESIAN_POINT('Ctrl Pts',(-0.15742340527262,0.146461291940682,
-0.612692181434314));
#37642=CARTESIAN_POINT('Ctrl Pts',(-0.208597246671037,-0.0521557737131904,
-0.601614300764492));
#37643=CARTESIAN_POINT('Ctrl Pts',(-0.0699682141387932,-0.203316210289885,
-0.590536420094669));
#37644=CARTESIAN_POINT('Ctrl Pts',(0.132324971798349,-0.169479016403749,
-0.579458539424848));
#37645=CARTESIAN_POINT('Ctrl Pts',(0.214215519316177,0.0185673331085495,
-0.568380658755025));
#37646=CARTESIAN_POINT('Ctrl Pts',(0.101191125174026,0.189719240784877,
-0.557302778085203));
#37647=CARTESIAN_POINT('Ctrl Pts',(-0.103907186618782,0.188245401321736,
-0.546224897415381));
#37648=CARTESIAN_POINT('Ctrl Pts',(-0.214460233207651,0.0154868591715072,
-0.535147016745558));
#37649=CARTESIAN_POINT('Ctrl Pts',(-0.129875673392626,-0.171363192803534,
-0.524069136075736));
#37650=CARTESIAN_POINT('Ctrl Pts',(0.0728829069770984,-0.202289684157425,
-0.512991255405913));
#37651=CARTESIAN_POINT('Ctrl Pts',(0.209325248727962,-0.0491525652461543,
-0.501913374736091));
#37652=CARTESIAN_POINT('Ctrl Pts',(0.155302312302862,0.148708527711963,
-0.490835494066269));
#37653=CARTESIAN_POINT('Ctrl Pts',(-0.0400303719398065,0.211259564875664,
-0.479757613396447));
#37654=CARTESIAN_POINT('Ctrl Pts',(-0.198939375944839,0.0815852874254244,
-0.468679732726624));
#37655=CARTESIAN_POINT('Ctrl Pts',(-0.176833219060973,-0.122323534374517,
-0.457601852056802));
#37656=CARTESIAN_POINT('Ctrl Pts',(0.0061736818113679,-0.214930035312299,
-0.446523971386979));
#37657=CARTESIAN_POINT('Ctrl Pts',(0.183563142692745,-0.111971456499662,
-0.435446090717158));
#37658=CARTESIAN_POINT('Ctrl Pts',(0.193928294537228,0.0928700759329271,
-0.424368210047335));
#37659=CARTESIAN_POINT('Ctrl Pts',(0.027837874078222,0.213209022306409,
-0.413290329377513));
#37660=CARTESIAN_POINT('Ctrl Pts',(-0.163582259169408,0.139548840593563,
-0.40221244870769));
#37661=CARTESIAN_POINT('Ctrl Pts',(-0.206158711667045,-0.0610869874011697,
-0.391134568037868));
#37662=CARTESIAN_POINT('Ctrl Pts',(-0.0611511216226529,-0.206139697172249,
-0.380056687368046));
#37663=CARTESIAN_POINT('Ctrl Pts',(0.139497942445576,-0.163625665711405,
-0.368978806698223));
#37664=CARTESIAN_POINT('Ctrl Pts',(0.213217672513124,0.0277715421608559,
-0.357900926028401));
#37665=CARTESIAN_POINT('Ctrl Pts',(0.0929304036628409,0.19389939272972,
-0.346823045358578));
#37666=CARTESIAN_POINT('Ctrl Pts',(-0.111914343517997,0.183597968783398,
-0.335745164688757));
#37667=CARTESIAN_POINT('Ctrl Pts',(-0.214928104240127,0.00624054749880152,
-0.324667284018934));
#37668=CARTESIAN_POINT('Ctrl Pts',(-0.122378542305555,-0.176795154935814,
-0.313589403349112));
#37669=CARTESIAN_POINT('Ctrl Pts',(0.0815233922863349,-0.1989647479812,
-0.302511522679289));
#37670=CARTESIAN_POINT('Ctrl Pts',(0.211247100952243,-0.0400960940759599,
-0.291433642009467));
#37671=CARTESIAN_POINT('Ctrl Pts',(0.148756836004253,0.155256040678952,
-0.280355761339645));
#37672=CARTESIAN_POINT('Ctrl Pts',(-0.0490874406258331,0.209340530281999,
-0.269277880669823));
#37673=CARTESIAN_POINT('Ctrl Pts',(-0.202266999948351,0.0729458368853433,
-0.2582));
#37674=CARTESIAN_POINT('Ctrl Pts',(-0.171403589822867,-0.129822354894342,
-0.247122119330178));
#37675=CARTESIAN_POINT('Ctrl Pts',(0.0154201390359869,-0.214465041118413,
-0.236044238660356));
#37676=CARTESIAN_POINT('Ctrl Pts',(0.188213065235466,-0.10396574538109,
-0.224966357990533));
#37677=CARTESIAN_POINT('Ctrl Pts',(0.189750714362162,0.101132096654386,
-0.213888477320711));
#37678=CARTESIAN_POINT('Ctrl Pts',(0.0186339728415945,0.214209734183008,
-0.202810596650889));
#37679=CARTESIAN_POINT('Ctrl Pts',(-0.169437835290407,0.13237768818239,
-0.191732715981066));
#37680=CARTESIAN_POINT('Ctrl Pts',(-0.203337979098878,-0.0699049519443599,
-0.180654835311244));
#37681=CARTESIAN_POINT('Ctrl Pts',(-0.052220645806835,-0.208581021946098,
-0.169576954641422));
#37682=CARTESIAN_POINT('Ctrl Pts',(0.14641226911824,-0.157468941020574,
-0.158499073971599));
#37683=CARTESIAN_POINT('Ctrl Pts',(0.211824577335415,0.0369242188441669,
-0.147421193301777));
#37684=CARTESIAN_POINT('Ctrl Pts',(0.084497311416599,0.197720155985876,
-0.136343312631954));
#37685=CARTESIAN_POINT('Ctrl Pts',(-0.119713859202124,0.178609986838626,
-0.125265431962133));
#37686=CARTESIAN_POINT('Ctrl Pts',(-0.214997814593688,-0.00301700913126643,
-0.11418755129231));
#37687=CARTESIAN_POINT('Ctrl Pts',(-0.114653952245116,-0.181899968541422,
-0.103109670622488));
#37688=CARTESIAN_POINT('Ctrl Pts',(0.0900116395095307,-0.195269764467508,
-0.0920317899526653));
#37689=CARTESIAN_POINT('Ctrl Pts',(0.21277940747491,-0.0309675335497962,
-0.0809539092828432));
#37690=CARTESIAN_POINT('Ctrl Pts',(0.141931585421943,0.161519998348358,
-0.0698760286130206));
#37691=CARTESIAN_POINT('Ctrl Pts',(-0.0580459054323005,0.207025236987341,
-0.0587981479431985));
#37692=CARTESIAN_POINT('Ctrl Pts',(-0.205234112760265,0.0641866881053908,
-0.047720267273376));
#37693=CARTESIAN_POINT('Ctrl Pts',(-0.165628585427786,-0.137110124877453,
-0.0366423866035538));
#37694=CARTESIAN_POINT('Ctrl Pts',(0.024585267046665,-0.213545749231955,
-0.0255645059337314));
#37695=CARTESIAN_POINT('Ctrl Pts',(0.192615845471205,-0.0958773620740437,
-0.0144866252639091));
#37696=CARTESIAN_POINT('Ctrl Pts',(0.185016024754682,0.109434141205358,
-0.00340874459408687));
#37697=CARTESIAN_POINT('Ctrl Pts',(0.068262639107798,0.179305101056521,
0.00397650918579475));
#37698=CARTESIAN_POINT('Ctrl Pts',(0.00795783122553719,0.181942719557458,
0.00766913607573553));
#37699=CARTESIAN_POINT('Ctrl Pts',(0.0980771099081362,-0.137424797458508,
-0.782269136075736));
#37700=CARTESIAN_POINT('Ctrl Pts',(0.143626478572908,-0.104917196796917,
-0.778576509185795));
#37701=CARTESIAN_POINT('Ctrl Pts',(0.199103118322308,0.00836770658400184,
-0.771191255405914));
#37702=CARTESIAN_POINT('Ctrl Pts',(0.101318206166701,0.171817038909262,
-0.76011337473609));
#37703=CARTESIAN_POINT('Ctrl Pts',(-0.0887389984301955,0.178429251393937,
-0.74903549406627));
#37704=CARTESIAN_POINT('Ctrl Pts',(-0.198008971104146,0.022939528150427,
-0.737957613396445));
#37705=CARTESIAN_POINT('Ctrl Pts',(-0.127133214698961,-0.153553308693652,
-0.726879732726626));
#37706=CARTESIAN_POINT('Ctrl Pts',(0.0594331939686611,-0.190259524094072,
-0.715801852056801));
#37707=CARTESIAN_POINT('Ctrl Pts',(0.191914975319761,-0.0538842134642793,
-0.70472397138698));
#37708=CARTESIAN_POINT('Ctrl Pts',(0.149776411252289,0.131539206486933,
-0.693646090717157));
#37709=CARTESIAN_POINT('Ctrl Pts',(-0.0286456120569251,0.197265086101302,
-0.682568210047335));
#37710=CARTESIAN_POINT('Ctrl Pts',(-0.181002050243358,0.0835044230570726,
-0.671490329377513));
#37711=CARTESIAN_POINT('Ctrl Pts',(-0.168664998254998,-0.106239726878691,
-0.66041244870769));
#37712=CARTESIAN_POINT('Ctrl Pts',(-0.0028592246550194,-0.199314803322844,
-0.649334568037868));
#37713=CARTESIAN_POINT('Ctrl Pts',(0.165548028979837,-0.111033866123113,
-0.638256687368046));
#37714=CARTESIAN_POINT('Ctrl Pts',(0.183323014829104,0.078277303315412,
-0.627178806698223));
#37715=CARTESIAN_POINT('Ctrl Pts',(0.0342921479767208,0.196363660480105,
-0.616100926028401));
#37716=CARTESIAN_POINT('Ctrl Pts',(-0.145941163669044,0.135778611454114,
-0.605023045358579));
#37717=CARTESIAN_POINT('Ctrl Pts',(-0.193382457104201,-0.0483516049889837,
-0.593945164688756));
#37718=CARTESIAN_POINT('Ctrl Pts',(-0.0648648310813553,-0.188486612083512,
-0.582867284018935));
#37719=CARTESIAN_POINT('Ctrl Pts',(0.122673374605773,-0.157117455492814,
-0.571789403349112));
#37720=CARTESIAN_POINT('Ctrl Pts',(0.19859094085045,0.0172130579655545,
-0.560711522679289));
#37721=CARTESIAN_POINT('Ctrl Pts',(0.0938103869326332,0.175881386396157,
-0.549633642009467));
#37722=CARTESIAN_POINT('Ctrl Pts',(-0.0963283426785271,0.174515046708994,
-0.538555761339645));
#37723=CARTESIAN_POINT('Ctrl Pts',(-0.19881780565512,0.0143572694616418,
-0.527477880669822));
#37724=CARTESIAN_POINT('Ctrl Pts',(-0.12040272457832,-0.15886420271802,
-0.516400000000001));
#37725=CARTESIAN_POINT('Ctrl Pts',(0.0675669303265321,-0.187534959322295,
-0.505322119330178));
#37726=CARTESIAN_POINT('Ctrl Pts',(0.194057359715773,-0.0455674463204479,
-0.494244238660356));
#37727=CARTESIAN_POINT('Ctrl Pts',(0.143974780235013,0.137861937011274,
-0.483166357990533));
#37728=CARTESIAN_POINT('Ctrl Pts',(-0.0371106129541729,0.195850589566256,
-0.472088477320711));
#37729=CARTESIAN_POINT('Ctrl Pts',(-0.1844290178751,0.075634571393753,-0.461010596650889));
#37730=CARTESIAN_POINT('Ctrl Pts',(-0.163935252959427,-0.113401427950385,
-0.449932715981066));
#37731=CARTESIAN_POINT('Ctrl Pts',(0.00572338214964429,-0.199253341055513,
-0.438854835311244));
#37732=CARTESIAN_POINT('Ctrl Pts',(0.170174305434017,-0.103804416064937,
-0.427776954641422));
#37733=CARTESIAN_POINT('Ctrl Pts',(0.17978343769215,0.0860962633111156,
-0.416699073971599));
#37734=CARTESIAN_POINT('Ctrl Pts',(0.0258074187253941,0.197657856315907,
-0.405621193301777));
#37735=CARTESIAN_POINT('Ctrl Pts',(-0.151650799431327,0.129370344578822,
-0.394543312631955));
#37736=CARTESIAN_POINT('Ctrl Pts',(-0.191121785411107,-0.0566313885214476,
-0.383465431962133));
#37737=CARTESIAN_POINT('Ctrl Pts',(-0.0566908448830847,-0.191104157806798,
-0.37238755129231));
#37738=CARTESIAN_POINT('Ctrl Pts',(0.12932315887011,-0.151691039961245,
-0.361309670622488));
#37739=CARTESIAN_POINT('Ctrl Pts',(0.19766587558872,0.0257459249647184,
-0.350231789952665));
#37740=CARTESIAN_POINT('Ctrl Pts',(0.0861521908213209,0.179756643941802,
-0.339153909282844));
#37741=CARTESIAN_POINT('Ctrl Pts',(-0.103751468823769,0.170206591358636,
-0.32807602861302));
#37742=CARTESIAN_POINT('Ctrl Pts',(-0.199251550833027,0.00578537074795013,
-0.316998147943199));
#37743=CARTESIAN_POINT('Ctrl Pts',(-0.113452423680357,-0.163899965177981,
-0.305920267273376));
#37744=CARTESIAN_POINT('Ctrl Pts',(0.0755771907989914,-0.184452539310841,
-0.294842386603554));
#37745=CARTESIAN_POINT('Ctrl Pts',(0.195839034743866,-0.0371715414102192,
-0.283764505933731));
#37746=CARTESIAN_POINT('Ctrl Pts',(0.137906721764718,0.143931883598223,
-0.272686625263909));
#37747=CARTESIAN_POINT('Ctrl Pts',(-0.04550707179827,0.194071526654768,
-0.261608744594087));
#37748=CARTESIAN_POINT('Ctrl Pts',(-0.187513929667502,0.0676252702158433,
-0.250530863924265));
#37749=CARTESIAN_POINT('Ctrl Pts',(-0.158901653235621,-0.120353295056254,
-0.239452983254442));
#37750=CARTESIAN_POINT('Ctrl Pts',(0.0142954157988977,-0.198822262883639,
-0.22837510258462));
#37751=CARTESIAN_POINT('Ctrl Pts',(0.174485069171344,-0.0963826302471343,
-0.217297221914798));
#37752=CARTESIAN_POINT('Ctrl Pts',(0.175910564335014,0.0937556638701326,
-0.206219341244975));
#37753=CARTESIAN_POINT('Ctrl Pts',(0.0172748370902665,0.198585577676752,
-0.195141460575153));
#37754=CARTESIAN_POINT('Ctrl Pts',(-0.157079278071916,0.12272224593096,
-0.184063579905331));
#37755=CARTESIAN_POINT('Ctrl Pts',(-0.188506793106217,-0.0648061831423422,
-0.172985699235508));
#37756=CARTESIAN_POINT('Ctrl Pts',(-0.0484117454034254,-0.193367415787862,
-0.161907818565686));
#37757=CARTESIAN_POINT('Ctrl Pts',(0.135733164287341,-0.145983378103634,
-0.150829937895864));
#37758=CARTESIAN_POINT('Ctrl Pts',(0.196374390812461,0.0342310182933485,
-0.139752057226041));
#37759=CARTESIAN_POINT('Ctrl Pts',(0.0783341964537513,0.183298726103865,
-0.128674176556219));
#37760=CARTESIAN_POINT('Ctrl Pts',(-0.11098209881189,0.165582425796218,
-0.117596295886397));
#37761=CARTESIAN_POINT('Ctrl Pts',(-0.199316176611518,-0.00279695273174133,
-0.106518415216575));
#37762=CARTESIAN_POINT('Ctrl Pts',(-0.106291254346392,-0.168632440864337,
-0.0954405345467521));
#37763=CARTESIAN_POINT('Ctrl Pts',(0.0834463172171277,-0.181027062693864,
-0.08436265387693));
#37764=CARTESIAN_POINT('Ctrl Pts',(0.197259576985525,-0.0287088052401784,
-0.0732847732071076));
#37765=CARTESIAN_POINT('Ctrl Pts',(0.131579295353188,0.149738957011886,
-0.0622068925372851));
#37766=CARTESIAN_POINT('Ctrl Pts',(-0.0538121187909959,0.191925107594194,
-0.051129011867463));
#37767=CARTESIAN_POINT('Ctrl Pts',(-0.190264625447194,0.0595050014192004,
-0.0400511311976405));
#37768=CARTESIAN_POINT('Ctrl Pts',(-0.153547869532668,-0.127109505354499,
-0.0289732505278182));
#37769=CARTESIAN_POINT('Ctrl Pts',(0.0227920522726021,-0.197970022853455,
-0.0178953698579958));
#37770=CARTESIAN_POINT('Ctrl Pts',(0.178566716813701,-0.088884202233921,
-0.00681748918817358));
#37771=CARTESIAN_POINT('Ctrl Pts',(0.17152121632332,0.101452168976872,0.00426039148164866));
#37772=CARTESIAN_POINT('Ctrl Pts',(0.0632836582924853,0.16622683936145,
0.0116456452615303));
#37773=CARTESIAN_POINT('Ctrl Pts',(0.0073773982167736,0.168672073681435,
0.0153382721514711));
#37774=CARTESIAN_POINT('Ctrl Pts',(0.0903606778650188,-0.126612599672285,
-0.7746));
#37775=CARTESIAN_POINT('Ctrl Pts',(0.132326349903352,-0.0966626058939412,
-0.77090737311006));
#37776=CARTESIAN_POINT('Ctrl Pts',(0.183438243169013,0.00770935888928891,
-0.763522119330179));
#37777=CARTESIAN_POINT('Ctrl Pts',(0.0933467737565466,0.158298955986194,
-0.752444238660355));
#37778=CARTESIAN_POINT('Ctrl Pts',(-0.0817572628182647,0.164390938130267,
-0.741366357990534));
#37779=CARTESIAN_POINT('Ctrl Pts',(-0.182430180386475,0.021134710387752,
-0.730288477320711));
#37780=CARTESIAN_POINT('Ctrl Pts',(-0.117130729791253,-0.141472164860598,
-0.719210596650888));
#37781=CARTESIAN_POINT('Ctrl Pts',(0.0547571568913644,-0.175290438141162,
-0.708132715981067));
#37782=CARTESIAN_POINT('Ctrl Pts',(0.176815643105561,-0.0496447546162005,
-0.697054835311244));
#37783=CARTESIAN_POINT('Ctrl Pts',(0.137992423121185,0.121190070497784,
-0.685976954641421));
#37784=CARTESIAN_POINT('Ctrl Pts',(-0.0263918556098016,0.181744822170133,
-0.6748990739716));
#37785=CARTESIAN_POINT('Ctrl Pts',(-0.166761316379197,0.0769345291600839,
-0.663821193301777));
#37786=CARTESIAN_POINT('Ctrl Pts',(-0.155394909053691,-0.0978810830166665,
-0.652743312631956));
#37787=CARTESIAN_POINT('Ctrl Pts',(-0.00263426887515189,-0.183633273387178,
-0.641665431962132));
#37788=CARTESIAN_POINT('Ctrl Pts',(0.15252317418251,-0.102298032825963,
-0.630587551292311));
#37789=CARTESIAN_POINT('Ctrl Pts',(0.168899673978284,0.0721186645451872,
-0.619509670622488));
#37790=CARTESIAN_POINT('Ctrl Pts',(0.0315941379137935,0.180914318189617,
-0.608431789952666));
#37791=CARTESIAN_POINT('Ctrl Pts',(-0.134458922065469,0.125095930967546,
-0.597353909282843));
#37792=CARTESIAN_POINT('Ctrl Pts',(-0.178167667537365,-0.0445474362647772,
-0.586276028613021));
#37793=CARTESIAN_POINT('Ctrl Pts',(-0.0597614480239172,-0.173657013877139,
-0.575198147943198));
#37794=CARTESIAN_POINT('Ctrl Pts',(0.113021777413197,-0.144755894581878,
-0.564120267273377));
#37795=CARTESIAN_POINT('Ctrl Pts',(0.182966362384724,0.0158587828225596,
-0.553042386603554));
#37796=CARTESIAN_POINT('Ctrl Pts',(0.0864296486912397,0.162043532007437,
-0.541964505933732));
#37797=CARTESIAN_POINT('Ctrl Pts',(-0.0887494987382724,0.160784692096253,
-0.53088662526391));
#37798=CARTESIAN_POINT('Ctrl Pts',(-0.18317537810259,0.0132276797517765,
-0.519808744594086));
#37799=CARTESIAN_POINT('Ctrl Pts',(-0.110929775764013,-0.146365212632506,
-0.508730863924265));
#37800=CARTESIAN_POINT('Ctrl Pts',(0.0622509536759654,-0.172780234487164,
-0.497652983254442));
#37801=CARTESIAN_POINT('Ctrl Pts',(0.178789470703585,-0.0419823273947417,
-0.48657510258462));
#37802=CARTESIAN_POINT('Ctrl Pts',(0.132647248167164,0.127015346310585,
-0.475497221914797));
#37803=CARTESIAN_POINT('Ctrl Pts',(-0.0341908539685392,0.180441614256847,
-0.464419341244976));
#37804=CARTESIAN_POINT('Ctrl Pts',(-0.169918659805362,0.069683855362082,
-0.453341460575152));
#37805=CARTESIAN_POINT('Ctrl Pts',(-0.15103728685788,-0.104479321526254,
-0.442263579905332));
#37806=CARTESIAN_POINT('Ctrl Pts',(0.00527308248792088,-0.183576646798727,
-0.431185699235508));
#37807=CARTESIAN_POINT('Ctrl Pts',(0.15678546817529,-0.0956373756302127,
-0.420107818565687));
#37808=CARTESIAN_POINT('Ctrl Pts',(0.165638580847071,0.079322450689304,
-0.409029937895864));
#37809=CARTESIAN_POINT('Ctrl Pts',(0.023776963372566,0.182106690325406,
-0.397952057226042));
#37810=CARTESIAN_POINT('Ctrl Pts',(-0.139719339693246,0.119191848564081,
-0.386874176556219));
#37811=CARTESIAN_POINT('Ctrl Pts',(-0.176084859155169,-0.0521757896417255,
-0.375796295886397));
#37812=CARTESIAN_POINT('Ctrl Pts',(-0.0522305681435164,-0.176068618441347,
-0.364718415216575));
#37813=CARTESIAN_POINT('Ctrl Pts',(0.119148375294644,-0.139756414211085,
-0.353640534546752));
#37814=CARTESIAN_POINT('Ctrl Pts',(0.182114078664316,0.023720307768581,
-0.34256265387693));
#37815=CARTESIAN_POINT('Ctrl Pts',(0.0793739779798006,0.165613895153883,
-0.331484773207108));
#37816=CARTESIAN_POINT('Ctrl Pts',(-0.0955885941295399,0.156815213933875,
-0.320406892537285));
#37817=CARTESIAN_POINT('Ctrl Pts',(-0.183574997425927,0.00533019399709877,
-0.309329011867463));
#37818=CARTESIAN_POINT('Ctrl Pts',(-0.10452630505516,-0.151004775420149,
-0.29825113119764));
#37819=CARTESIAN_POINT('Ctrl Pts',(0.0696309893116479,-0.169940330640481,
-0.287173250527819));
#37820=CARTESIAN_POINT('Ctrl Pts',(0.180430968535489,-0.0342469887444786,
-0.276095369857996));
#37821=CARTESIAN_POINT('Ctrl Pts',(0.127056607525184,0.132607726517495,
-0.265017489188174));
#37822=CARTESIAN_POINT('Ctrl Pts',(-0.0419267029707069,0.178802523027537,
-0.253939608518351));
#37823=CARTESIAN_POINT('Ctrl Pts',(-0.172760859386654,0.0623047035463433,
-0.242861727848529));
#37824=CARTESIAN_POINT('Ctrl Pts',(-0.146399716648376,-0.110884235218166,
-0.231783847178707));
#37825=CARTESIAN_POINT('Ctrl Pts',(0.0131706925618085,-0.183179484648865,
-0.220705966508885));
#37826=CARTESIAN_POINT('Ctrl Pts',(0.160757073107222,-0.0887995151131783,
-0.209628085839062));
#37827=CARTESIAN_POINT('Ctrl Pts',(0.162070414307866,0.0863792310858789,
-0.19855020516924));
#37828=CARTESIAN_POINT('Ctrl Pts',(0.0159157013389389,0.182961421170497,
-0.187472324499417));
#37829=CARTESIAN_POINT('Ctrl Pts',(-0.144720720853425,0.113066803679531,
-0.176394443829595));
#37830=CARTESIAN_POINT('Ctrl Pts',(-0.173675607113556,-0.0597074143403244,
-0.165316563159773));
#37831=CARTESIAN_POINT('Ctrl Pts',(-0.044602845000016,-0.178153809629627,
-0.15423868248995));
#37832=CARTESIAN_POINT('Ctrl Pts',(0.125054059456442,-0.134497815186694,
-0.143160801820128));
#37833=CARTESIAN_POINT('Ctrl Pts',(0.180924204289506,0.0315378177425299,
-0.132082921150306));
#37834=CARTESIAN_POINT('Ctrl Pts',(0.0721710814909035,0.168877296221853,
-0.121005040480484));
#37835=CARTESIAN_POINT('Ctrl Pts',(-0.102250338421656,0.15255486475381,
-0.109927159810661));
#37836=CARTESIAN_POINT('Ctrl Pts',(-0.183634538629348,-0.00257689633221619,
-0.098849279140839));
#37837=CARTESIAN_POINT('Ctrl Pts',(-0.0979285564476671,-0.155364913187252,
-0.0877713984710165));
#37838=CARTESIAN_POINT('Ctrl Pts',(0.0768809949247246,-0.16678436092022,
-0.0766935178011943));
#37839=CARTESIAN_POINT('Ctrl Pts',(0.181739746496141,-0.0264500769305604,
-0.0656156371313721));
#37840=CARTESIAN_POINT('Ctrl Pts',(0.121227005284432,0.137957915675413,
-0.0545377564615496));
#37841=CARTESIAN_POINT('Ctrl Pts',(-0.0495783321496912,0.176824978201047,
-0.0434598757917274));
#37842=CARTESIAN_POINT('Ctrl Pts',(-0.175295138134123,0.0548233147330098,
-0.0323819951219049));
#37843=CARTESIAN_POINT('Ctrl Pts',(-0.141467153637551,-0.117108885831544,
-0.0213041144520827));
#37844=CARTESIAN_POINT('Ctrl Pts',(0.0209988374985395,-0.182394296474955,
-0.0102262337822603));
#37845=CARTESIAN_POINT('Ctrl Pts',(0.164517588156196,-0.0818910423937984,
0.000851646887561965));
#37846=CARTESIAN_POINT('Ctrl Pts',(0.158026407891959,0.0934701967483867,
0.0119295275573842));
#37847=CARTESIAN_POINT('Ctrl Pts',(0.0583046774771726,0.153148577666378,
0.0193147813372658));
#37848=CARTESIAN_POINT('Ctrl Pts',(0.00679696520801,0.155401427805413,0.0230074082272066));
#37849=CARTESIAN_POINT('',(0.00853826423430079,0.19521336543348,0.));
#37850=CARTESIAN_POINT('Ctrl Pts',(0.133815347598873,-0.0797905857758447,
1.28369537222284E-16));
#37851=CARTESIAN_POINT('Ctrl Pts',(0.136293565210637,-0.0766448939156863,
1.28593437618207E-16));
#37852=CARTESIAN_POINT('Ctrl Pts',(0.138637419022965,-0.0734038133327389,
7.54322313592872E-17));
#37853=CARTESIAN_POINT('Ctrl Pts',(0.140838976075351,-0.0700729779668307,
7.63278329429795E-17));
#37854=CARTESIAN_POINT('Ctrl Pts',(0.145819973356658,-0.0625370016067841,
7.81008351086913E-17));
#37855=CARTESIAN_POINT('Ctrl Pts',(0.150074011938905,-0.054542919364199,
-1.3346458730469E-16));
#37856=CARTESIAN_POINT('Ctrl Pts',(0.153617808369117,-0.046201435097827,
-1.04083408558608E-16));
#37857=CARTESIAN_POINT('Ctrl Pts',(0.155065400881004,-0.0427940525351372,
-9.20815977376891E-17));
#37858=CARTESIAN_POINT('Ctrl Pts',(0.156393229106788,-0.0393303545681794,
2.29694749575199E-16));
#37859=CARTESIAN_POINT('Ctrl Pts',(0.157599445512596,-0.0358262975538223,
1.6306400674182E-16));
#37860=CARTESIAN_POINT('Ctrl Pts',(0.160399820179621,-0.0276912129640526,
8.37282249230137E-18));
#37861=CARTESIAN_POINT('Ctrl Pts',(0.162551197740732,-0.0193269206951015,
-2.31903545997953E-16));
#37862=CARTESIAN_POINT('Ctrl Pts',(0.164064259316912,-0.0108223648054157,
-2.81025203108243E-16));
#37863=CARTESIAN_POINT('Ctrl Pts',(0.165045137245379,-0.00530908544195027,
-3.12869478336516E-16));
#37864=CARTESIAN_POINT('Ctrl Pts',(0.165757428744978,0.000269613978694174,
-5.88307172475674E-18));
#37865=CARTESIAN_POINT('Ctrl Pts',(0.166199326803605,0.00585654216766985,
-3.46944695195361E-18));
#37866=CARTESIAN_POINT('Ctrl Pts',(0.167121638500691,0.0175173519831342,
1.56817273628343E-18));
#37867=CARTESIAN_POINT('Ctrl Pts',(0.166875568718661,0.029234254531895,
-1.25050453494893E-16));
#37868=CARTESIAN_POINT('Ctrl Pts',(0.165478560136187,0.0408032009544139,
-1.09287578986539E-16));
#37869=CARTESIAN_POINT('Ctrl Pts',(0.164815426560599,0.0462947612090889,
-1.01805240319898E-16));
#37870=CARTESIAN_POINT('Ctrl Pts',(0.163892264719358,0.0517533269403495,
-1.02393347651096E-16));
#37871=CARTESIAN_POINT('Ctrl Pts',(0.16270697339196,0.0571579380710028,
-9.0205620750794E-17));
#37872=CARTESIAN_POINT('Ctrl Pts',(0.161749752444841,0.0615226093258332,
-8.03630215373626E-17));
#37873=CARTESIAN_POINT('Ctrl Pts',(0.160620157616345,0.0658551527740701,
-8.55423955822509E-17));
#37874=CARTESIAN_POINT('Ctrl Pts',(0.159324513207994,0.0701199726232436,
-6.59194920871187E-17));
#37875=CARTESIAN_POINT('Ctrl Pts',(0.15729280825055,0.0768076529576913,
-3.51487419850738E-17));
#37876=CARTESIAN_POINT('Ctrl Pts',(0.154851112214637,0.0833408692938153,
-2.23469952887909E-17));
#37877=CARTESIAN_POINT('Ctrl Pts',(0.152001406717412,0.0896785574668918,
4.85722573273506E-17));
#37878=CARTESIAN_POINT('Ctrl Pts',(0.148854441839518,0.096677344572132,
1.26781386779886E-16));
#37879=CARTESIAN_POINT('Ctrl Pts',(0.145210141356519,0.103437941488835,
9.23711880014318E-17));
#37880=CARTESIAN_POINT('Ctrl Pts',(0.141116132135723,0.109938863795627,
1.56125112837913E-16));
#37881=CARTESIAN_POINT('Ctrl Pts',(0.13847980310281,0.114125119686566,1.97179324966914E-16));
#37882=CARTESIAN_POINT('Ctrl Pts',(0.135656780122337,0.118203658930518,
-1.03755060408231E-16));
#37883=CARTESIAN_POINT('Ctrl Pts',(0.132657783307425,0.122167988997596,
-5.55111512312578E-17));
#37884=CARTESIAN_POINT('Ctrl Pts',(0.130633788308025,0.124843478411871,
-2.29517865663081E-17));
#37885=CARTESIAN_POINT('Ctrl Pts',(0.128531392348119,0.127464306685902,
-6.25671501750493E-17));
#37886=CARTESIAN_POINT('Ctrl Pts',(0.126360131478195,0.13002209138432,-6.07153216591882E-17));
#37887=CARTESIAN_POINT('Ctrl Pts',(0.118964139957754,0.138734703582444,
-5.44074163354499E-17));
#37888=CARTESIAN_POINT('Ctrl Pts',(0.110754606049639,0.146740382010002,
7.59358561344913E-17));
#37889=CARTESIAN_POINT('Ctrl Pts',(0.101878988500282,0.153971613547104,
-1.90819582357449E-17));
#37890=CARTESIAN_POINT('Ctrl Pts',(0.0962401643390006,0.158565732534371,
-7.94483208514698E-17));
#37891=CARTESIAN_POINT('Ctrl Pts',(0.0903316376136661,0.16284704475175,
-2.22921060177516E-16));
#37892=CARTESIAN_POINT('Ctrl Pts',(0.0841843402892172,0.166793948755328,
-2.33320307518881E-16));
#37893=CARTESIAN_POINT('Ctrl Pts',(0.0800454559343232,0.169451340836512,
-2.40321966923358E-16));
#37894=CARTESIAN_POINT('Ctrl Pts',(0.0757941213185356,0.171958832063456,
-8.02031543966986E-17));
#37895=CARTESIAN_POINT('Ctrl Pts',(0.0714649579678027,0.174295835998696,
-8.28330459778925E-17));
#37896=CARTESIAN_POINT('Ctrl Pts',(0.0601793857165482,0.18038810478734,
-8.96888352027333E-17));
#37897=CARTESIAN_POINT('Ctrl Pts',(0.0483399292857095,0.185344713462473,
-1.08355695937117E-16));
#37898=CARTESIAN_POINT('Ctrl Pts',(0.0361201977079082,0.189063915695687,
-1.57859836313889E-16));
#37899=CARTESIAN_POINT('Ctrl Pts',(0.0271139376768322,0.191805064485021,
-1.94345675467512E-16));
#37900=CARTESIAN_POINT('Ctrl Pts',(0.0179000121429095,0.193873604321062,
-1.33645313566251E-16));
#37901=CARTESIAN_POINT('Ctrl Pts',(0.00853826423430357,0.19521336543348,
-1.57859836313889E-16));
#37902=CARTESIAN_POINT('Ctrl Pts',(0.00853826423430082,0.19521336543348,
-1.73472347597681E-18));
#37903=CARTESIAN_POINT('Ctrl Pts',(0.0732416199231104,0.192383362751592,
-0.00369262688994077));
#37904=CARTESIAN_POINT('Ctrl Pts',(0.135876226554577,0.154899738092718,
-0.00738525377988161));
#37905=CARTESIAN_POINT('Ctrl Pts',(0.168552553360754,0.0994434865386125,
-0.0110778806698224));
#37906=CARTESIAN_POINT('Ctrl Pts',(0.201228880166931,0.043987234984507,
-0.0147705075597632));
#37907=CARTESIAN_POINT('Ctrl Pts',(0.20394692714782,-0.0294416434648305,
-0.018463134449704));
#37908=CARTESIAN_POINT('Ctrl Pts',(0.175258201920267,-0.087197908305547,
-0.0221557613396447));
#37909=CARTESIAN_POINT('Ctrl Pts',(0.146569476692714,-0.144954173146263,
-0.0258483882295855));
#37910=CARTESIAN_POINT('Ctrl Pts',(0.0864739792567223,-0.187037824378359,
-0.0295410151195261));
#37911=CARTESIAN_POINT('Ctrl Pts',(0.022411600014787,-0.194411194792733,
-0.0332336420094669));
#37912=CARTESIAN_POINT('Ctrl Pts',(-0.0416507792271474,-0.201784565207106,
-0.0369262688994076));
#37913=CARTESIAN_POINT('Ctrl Pts',(-0.109680040275024,-0.174447654803758,
-0.0406188957893484));
#37914=CARTESIAN_POINT('Ctrl Pts',(-0.150777053924035,-0.124782679736753,
-0.0443115226792891));
#37915=CARTESIAN_POINT('Ctrl Pts',(-0.179348311665281,-0.0902548472409218,
-0.0468786920487183));
#37916=CARTESIAN_POINT('Ctrl Pts',(-0.194902573031226,-0.0449353295028645,
-0.0494458614181474));
#37917=CARTESIAN_POINT('Ctrl Pts',(-0.195265563427387,0.000160747932399612,
-0.0520130307875765));
#37918=CARTESIAN_POINT('Origin',(0.324759526419164,-0.1875,0.5));
#37919=CARTESIAN_POINT('',(0.324759526419164,-0.1875,0.475));
#37920=CARTESIAN_POINT('',(0.352933712456347,-0.188249288476161,0.45));
#37921=CARTESIAN_POINT('Ctrl Pts',(0.324759526419164,-0.1875,0.475));
#37922=CARTESIAN_POINT('Ctrl Pts',(0.33839219708232,-0.187862558940078,
0.463012481414242));
#37923=CARTESIAN_POINT('Ctrl Pts',(0.352933712456347,-0.188249288476161,
0.45));
#37924=CARTESIAN_POINT('',(0.324759526419164,-0.1875,0.015));
#37925=CARTESIAN_POINT('',(0.324759526419164,-0.1875,0.5));
#37926=CARTESIAN_POINT('',(0.352933712456347,-0.188249288476161,0.04));
#37927=CARTESIAN_POINT('Ctrl Pts',(0.352933712456347,-0.188249288476161,
0.04));
#37928=CARTESIAN_POINT('Ctrl Pts',(0.338392197082319,-0.187862558940078,
0.0269875185857579));
#37929=CARTESIAN_POINT('Ctrl Pts',(0.324759526419164,-0.1875,0.015));
#37930=CARTESIAN_POINT('',(0.352933712456347,-0.188249288476161,0.245));
#37931=CARTESIAN_POINT('Origin',(0.362615522993687,-0.249218744246926,0.5));
#37932=CARTESIAN_POINT('',(0.339495522292874,-0.211524916601068,0.45));
#37933=CARTESIAN_POINT('Ctrl Pts',(0.339495522292874,-0.211524916601068,
0.45));
#37934=CARTESIAN_POINT('Ctrl Pts',(0.331889847003218,-0.19912495964568,
0.463012481414243));
#37935=CARTESIAN_POINT('Ctrl Pts',(0.324759526419164,-0.1875,0.475));
#37936=CARTESIAN_POINT('',(0.339495522292874,-0.211524916601068,0.04));
#37937=CARTESIAN_POINT('',(0.339495522292874,-0.211524916601068,0.245));
#37938=CARTESIAN_POINT('Ctrl Pts',(0.324759526419164,-0.1875,0.015));
#37939=CARTESIAN_POINT('Ctrl Pts',(0.331889847003216,-0.199124959645677,
0.0269875185857545));
#37940=CARTESIAN_POINT('Ctrl Pts',(0.339495522292874,-0.211524916601068,
0.04));
#37941=CARTESIAN_POINT('Origin',(0.1875,-0.324759526419164,0.5));
#37942=CARTESIAN_POINT('',(0.1875,-0.324759526419164,0.475));
#37943=CARTESIAN_POINT('',(0.211524916601068,-0.339495522292874,0.45));
#37944=CARTESIAN_POINT('Ctrl Pts',(0.1875,-0.324759526419164,0.475));
#37945=CARTESIAN_POINT('Ctrl Pts',(0.199124959645676,-0.331889847003216,
0.463012481414246));
#37946=CARTESIAN_POINT('Ctrl Pts',(0.211524916601068,-0.339495522292874,
0.45));
#37947=CARTESIAN_POINT('',(0.1875,-0.324759526419164,0.0150000000000001));
#37948=CARTESIAN_POINT('',(0.1875,-0.324759526419164,0.5));
#37949=CARTESIAN_POINT('',(0.211524916601068,-0.339495522292874,0.04));
#37950=CARTESIAN_POINT('Ctrl Pts',(0.211524916601068,-0.339495522292874,
0.04));
#37951=CARTESIAN_POINT('Ctrl Pts',(0.19912495964567,-0.331889847003212,
0.0269875185857474));
#37952=CARTESIAN_POINT('Ctrl Pts',(0.1875,-0.324759526419164,0.0150000000000001));
#37953=CARTESIAN_POINT('',(0.211524916601068,-0.339495522292874,0.245));
#37954=CARTESIAN_POINT('Origin',(0.18942488259565,-0.397137525113939,0.5));
#37955=CARTESIAN_POINT('',(0.188249288476161,-0.352933712456347,0.45));
#37956=CARTESIAN_POINT('Ctrl Pts',(0.188249288476161,-0.352933712456347,
0.45));
#37957=CARTESIAN_POINT('Ctrl Pts',(0.187862558940078,-0.338392197082316,
0.463012481414245));
#37958=CARTESIAN_POINT('Ctrl Pts',(0.1875,-0.324759526419164,0.475));
#37959=CARTESIAN_POINT('',(0.188249288476161,-0.352933712456347,0.04));
#37960=CARTESIAN_POINT('',(0.188249288476161,-0.352933712456347,0.245));
#37961=CARTESIAN_POINT('Ctrl Pts',(0.1875,-0.324759526419164,0.0150000000000001));
#37962=CARTESIAN_POINT('Ctrl Pts',(0.187862558940078,-0.338392197082329,
0.0269875185857667));
#37963=CARTESIAN_POINT('Ctrl Pts',(0.188249288476161,-0.352933712456347,
0.04));
#37964=CARTESIAN_POINT('Origin',(-6.88863824520386E-17,-0.375,0.5));
#37965=CARTESIAN_POINT('',(-6.88863824520386E-17,-0.375,0.475));
#37966=CARTESIAN_POINT('',(0.013438190163473,-0.399774205077229,0.45));
#37967=CARTESIAN_POINT('Ctrl Pts',(-6.88863824520386E-17,-0.375,0.475));
#37968=CARTESIAN_POINT('Ctrl Pts',(0.00650235007909994,-0.386987518585756,
0.463012481414244));
#37969=CARTESIAN_POINT('Ctrl Pts',(0.013438190163473,-0.399774205077229,
0.45));
#37970=CARTESIAN_POINT('',(-6.88863824520386E-17,-0.375,0.015));
#37971=CARTESIAN_POINT('',(-6.88863824520386E-17,-0.375,0.5));
#37972=CARTESIAN_POINT('',(0.013438190163473,-0.399774205077229,0.04));
#37973=CARTESIAN_POINT('Ctrl Pts',(0.013438190163473,-0.399774205077229,
0.04));
#37974=CARTESIAN_POINT('Ctrl Pts',(0.00650235007910186,-0.38698751858576,
0.0269875185857598));
#37975=CARTESIAN_POINT('Ctrl Pts',(-6.88863824520386E-17,-0.375,0.015));
#37976=CARTESIAN_POINT('',(0.013438190163473,-0.399774205077229,0.245));
#37977=CARTESIAN_POINT('Origin',(-0.0345220021202517,-0.438643626842576,
0.5));
#37978=CARTESIAN_POINT('',(-0.013438190163473,-0.399774205077229,0.45));
#37979=CARTESIAN_POINT('Ctrl Pts',(-0.013438190163473,-0.399774205077229,
0.45));
#37980=CARTESIAN_POINT('Ctrl Pts',(-0.00650235007910025,-0.386987518585757,
0.463012481414243));
#37981=CARTESIAN_POINT('Ctrl Pts',(-6.88863824520386E-17,-0.375,0.475));
#37982=CARTESIAN_POINT('',(-0.013438190163473,-0.399774205077229,0.04));
#37983=CARTESIAN_POINT('',(-0.013438190163473,-0.399774205077229,0.245));
#37984=CARTESIAN_POINT('Ctrl Pts',(-6.88863824520386E-17,-0.375,0.015));
#37985=CARTESIAN_POINT('Ctrl Pts',(-0.00650235007910422,-0.386987518585764,
0.0269875185857641));
#37986=CARTESIAN_POINT('Ctrl Pts',(-0.013438190163473,-0.399774205077229,
0.04));
#37987=CARTESIAN_POINT('Origin',(-0.1875,-0.324759526419164,0.5));
#37988=CARTESIAN_POINT('',(-0.1875,-0.324759526419164,0.475));
#37989=CARTESIAN_POINT('',(-0.188249288476161,-0.352933712456347,0.45));
#37990=CARTESIAN_POINT('Ctrl Pts',(-0.1875,-0.324759526419164,0.475));
#37991=CARTESIAN_POINT('Ctrl Pts',(-0.187862558940078,-0.33839219708232,
0.463012481414242));
#37992=CARTESIAN_POINT('Ctrl Pts',(-0.188249288476161,-0.352933712456347,
0.45));
#37993=CARTESIAN_POINT('',(-0.1875,-0.324759526419164,0.015));
#37994=CARTESIAN_POINT('',(-0.1875,-0.324759526419164,0.5));
#37995=CARTESIAN_POINT('',(-0.188249288476161,-0.352933712456347,0.04));
#37996=CARTESIAN_POINT('Ctrl Pts',(-0.188249288476161,-0.352933712456347,
0.04));
#37997=CARTESIAN_POINT('Ctrl Pts',(-0.187862558940078,-0.338392197082319,
0.0269875185857579));
#37998=CARTESIAN_POINT('Ctrl Pts',(-0.1875,-0.324759526419164,0.015));
#37999=CARTESIAN_POINT('',(-0.188249288476161,-0.352933712456347,0.245));
#38000=CARTESIAN_POINT('Origin',(-0.249218744246926,-0.362615522993687,
0.5));
#38001=CARTESIAN_POINT('',(-0.211524916601068,-0.339495522292874,0.45));
#38002=CARTESIAN_POINT('Ctrl Pts',(-0.211524916601068,-0.339495522292874,
0.45));
#38003=CARTESIAN_POINT('Ctrl Pts',(-0.199124959645674,-0.331889847003215,
0.463012481414248));
#38004=CARTESIAN_POINT('Ctrl Pts',(-0.1875,-0.324759526419164,0.475));
#38005=CARTESIAN_POINT('',(-0.211524916601068,-0.339495522292874,0.04));
#38006=CARTESIAN_POINT('',(-0.211524916601068,-0.339495522292874,0.245));
#38007=CARTESIAN_POINT('Ctrl Pts',(-0.1875,-0.324759526419164,0.015));
#38008=CARTESIAN_POINT('Ctrl Pts',(-0.199124959645673,-0.331889847003214,
0.0269875185857501));
#38009=CARTESIAN_POINT('Ctrl Pts',(-0.211524916601068,-0.339495522292874,
0.04));
#38010=CARTESIAN_POINT('Origin',(-0.324759526419164,-0.1875,0.5));
#38011=CARTESIAN_POINT('',(-0.324759526419164,-0.1875,0.475));
#38012=CARTESIAN_POINT('',(-0.339495522292874,-0.211524916601068,0.45));
#38013=CARTESIAN_POINT('Ctrl Pts',(-0.324759526419164,-0.1875,0.475));
#38014=CARTESIAN_POINT('Ctrl Pts',(-0.331889847003216,-0.199124959645676,
0.463012481414247));
#38015=CARTESIAN_POINT('Ctrl Pts',(-0.339495522292874,-0.211524916601068,
0.45));
#38016=CARTESIAN_POINT('',(-0.324759526419164,-0.1875,0.0150000000000001));
#38017=CARTESIAN_POINT('',(-0.324759526419164,-0.1875,0.5));
#38018=CARTESIAN_POINT('',(-0.339495522292874,-0.211524916601068,0.04));
#38019=CARTESIAN_POINT('Ctrl Pts',(-0.339495522292874,-0.211524916601068,
0.04));
#38020=CARTESIAN_POINT('Ctrl Pts',(-0.331889847003214,-0.199124959645674,
0.0269875185857514));
#38021=CARTESIAN_POINT('Ctrl Pts',(-0.324759526419164,-0.1875,0.0150000000000001));
#38022=CARTESIAN_POINT('',(-0.339495522292874,-0.211524916601068,0.245));
#38023=CARTESIAN_POINT('Origin',(-0.397137525113939,-0.18942488259565,0.5));
#38024=CARTESIAN_POINT('',(-0.352933712456347,-0.188249288476161,0.45));
#38025=CARTESIAN_POINT('Ctrl Pts',(-0.352933712456347,-0.188249288476161,
0.45));
#38026=CARTESIAN_POINT('Ctrl Pts',(-0.338392197082316,-0.187862558940078,
0.463012481414245));
#38027=CARTESIAN_POINT('Ctrl Pts',(-0.324759526419164,-0.1875,0.475));
#38028=CARTESIAN_POINT('',(-0.352933712456347,-0.188249288476161,0.04));
#38029=CARTESIAN_POINT('',(-0.352933712456347,-0.188249288476161,0.245));
#38030=CARTESIAN_POINT('Ctrl Pts',(-0.324759526419165,-0.1875,0.0150000000000001));
#38031=CARTESIAN_POINT('Ctrl Pts',(-0.338392197082305,-0.187862558940078,
0.0269875185857457));
#38032=CARTESIAN_POINT('Ctrl Pts',(-0.352933712456347,-0.188249288476161,
0.04));
#38033=CARTESIAN_POINT('Origin',(-0.375,4.59242549680257E-17,0.5));
#38034=CARTESIAN_POINT('',(-0.375,4.59242549680257E-17,0.475));
#38035=CARTESIAN_POINT('',(-0.399774205077229,-0.0134381901634729,0.45));
#38036=CARTESIAN_POINT('Ctrl Pts',(-0.375,4.59242549680257E-17,0.475));
#38037=CARTESIAN_POINT('Ctrl Pts',(-0.386987518585757,-0.00650235007910003,
0.463012481414244));
#38038=CARTESIAN_POINT('Ctrl Pts',(-0.399774205077229,-0.0134381901634728,
0.45));
#38039=CARTESIAN_POINT('',(-0.375,4.59242549680257E-17,0.015));
#38040=CARTESIAN_POINT('',(-0.375,4.59242549680257E-17,0.5));
#38041=CARTESIAN_POINT('',(-0.399774205077229,-0.0134381901634729,0.04));
#38042=CARTESIAN_POINT('Ctrl Pts',(-0.399774205077229,-0.0134381901634728,
0.04));
#38043=CARTESIAN_POINT('Ctrl Pts',(-0.386987518585752,-0.00650235007909753,
0.0269875185857518));
#38044=CARTESIAN_POINT('Ctrl Pts',(-0.375,4.59242549680257E-17,0.015));
#38045=CARTESIAN_POINT('',(-0.399774205077229,-0.0134381901634729,0.245));
#38046=CARTESIAN_POINT('Origin',(-0.438643626842576,0.0345220021202518,
0.5));
#38047=CARTESIAN_POINT('',(-0.399774205077229,0.013438190163473,0.45));
#38048=CARTESIAN_POINT('Ctrl Pts',(-0.399774205077229,0.013438190163473,
0.45));
#38049=CARTESIAN_POINT('Ctrl Pts',(-0.38698751858575,0.00650235007909647,
0.46301248141425));
#38050=CARTESIAN_POINT('Ctrl Pts',(-0.375,4.59242549680257E-17,0.475));
#38051=CARTESIAN_POINT('',(-0.399774205077229,0.013438190163473,0.04));
#38052=CARTESIAN_POINT('',(-0.399774205077229,0.013438190163473,0.245));
#38053=CARTESIAN_POINT('Ctrl Pts',(-0.375,4.59242549680257E-17,0.015));
#38054=CARTESIAN_POINT('Ctrl Pts',(-0.386987518585749,0.00650235007909624,
0.0269875185857492));
#38055=CARTESIAN_POINT('Ctrl Pts',(-0.399774205077229,0.013438190163473,
0.04));
#38056=CARTESIAN_POINT('Origin',(-0.362222184858401,0.0970571419134454,
0.5));
#38057=CARTESIAN_POINT('',(-0.362222184858401,0.0970571419134454,0.475));
#38058=CARTESIAN_POINT('',(-0.389630288914294,0.0904888830772256,0.45));
#38059=CARTESIAN_POINT('Ctrl Pts',(-0.362222184858401,0.0970571419134454,
0.475));
#38060=CARTESIAN_POINT('Ctrl Pts',(-0.375484170691896,0.0938789521539844,
0.463012481414245));
#38061=CARTESIAN_POINT('Ctrl Pts',(-0.389630288914294,0.0904888830772256,
0.45));
#38062=CARTESIAN_POINT('',(-0.362222184858401,0.0970571419134454,0.015));
#38063=CARTESIAN_POINT('',(-0.362222184858401,0.0970571419134454,0.5));
#38064=CARTESIAN_POINT('',(-0.389630288914294,0.0904888830772256,0.04));
#38065=CARTESIAN_POINT('Ctrl Pts',(-0.389630288914294,0.0904888830772256,
0.04));
#38066=CARTESIAN_POINT('Ctrl Pts',(-0.375484170691898,0.093878952153984,
0.0269875185857566));
#38067=CARTESIAN_POINT('Ctrl Pts',(-0.362222184858401,0.0970571419134454,
0.015));
#38068=CARTESIAN_POINT('',(-0.389630288914294,0.0904888830772256,0.245));
#38069=CARTESIAN_POINT('Origin',(-0.414762256080559,0.146875018062859,0.5));
#38070=CARTESIAN_POINT('',(-0.382674169822262,0.11644947295219,0.45));
#38071=CARTESIAN_POINT('Ctrl Pts',(-0.382674169822262,0.11644947295219,
0.45));
#38072=CARTESIAN_POINT('Ctrl Pts',(-0.372118306615107,0.106440527899934,
0.463012481414244));
#38073=CARTESIAN_POINT('Ctrl Pts',(-0.362222184858401,0.0970571419134454,
0.475));
#38074=CARTESIAN_POINT('',(-0.382674169822262,0.11644947295219,0.04));
#38075=CARTESIAN_POINT('',(-0.382674169822262,0.11644947295219,0.245));
#38076=CARTESIAN_POINT('Ctrl Pts',(-0.362222184858401,0.0970571419134454,
0.015));
#38077=CARTESIAN_POINT('Ctrl Pts',(-0.372118306615099,0.106440527899927,
0.026987518585746));
#38078=CARTESIAN_POINT('Ctrl Pts',(-0.382674169822262,0.11644947295219,
0.04));
#38079=CARTESIAN_POINT('Origin',(-0.265165042944955,0.265165042944955,0.5));
#38080=CARTESIAN_POINT('',(-0.265165042944955,0.265165042944955,0.475));
#38081=CARTESIAN_POINT('',(-0.292185286745036,0.273180815962104,0.45));
#38082=CARTESIAN_POINT('Ctrl Pts',(-0.265165042944955,0.265165042944955,
0.475));
#38083=CARTESIAN_POINT('Ctrl Pts',(-0.278239354461118,0.269043642791961,
0.463012481414249));
#38084=CARTESIAN_POINT('Ctrl Pts',(-0.292185286745036,0.273180815962104,
0.45));
#38085=CARTESIAN_POINT('',(-0.265165042944955,0.265165042944955,0.015));
#38086=CARTESIAN_POINT('',(-0.265165042944955,0.265165042944955,0.5));
#38087=CARTESIAN_POINT('',(-0.292185286745036,0.273180815962104,0.04));
#38088=CARTESIAN_POINT('Ctrl Pts',(-0.292185286745036,0.273180815962104,
0.04));
#38089=CARTESIAN_POINT('Ctrl Pts',(-0.278239354461119,0.269043642791962,
0.026987518585752));
#38090=CARTESIAN_POINT('Ctrl Pts',(-0.265165042944955,0.265165042944955,
0.015));
#38091=CARTESIAN_POINT('',(-0.292185286745036,0.273180815962104,0.245));
#38092=CARTESIAN_POINT('Origin',(-0.285757141265281,0.334578624864014,0.5));
#38093=CARTESIAN_POINT('',(-0.273180815962104,0.292185286745036,0.45));
#38094=CARTESIAN_POINT('Ctrl Pts',(-0.273180815962104,0.292185286745036,
0.45));
#38095=CARTESIAN_POINT('Ctrl Pts',(-0.26904364279196,0.278239354461116,
0.463012481414251));
#38096=CARTESIAN_POINT('Ctrl Pts',(-0.265165042944955,0.265165042944955,
0.475));
#38097=CARTESIAN_POINT('',(-0.273180815962104,0.292185286745036,0.04));
#38098=CARTESIAN_POINT('',(-0.273180815962104,0.292185286745036,0.245));
#38099=CARTESIAN_POINT('Ctrl Pts',(-0.265165042944955,0.265165042944955,
0.015));
#38100=CARTESIAN_POINT('Ctrl Pts',(-0.269043642791957,0.278239354461105,
0.0269875185857388));
#38101=CARTESIAN_POINT('Ctrl Pts',(-0.273180815962104,0.292185286745036,
0.04));
#38102=CARTESIAN_POINT('Origin',(-0.0970571419134453,0.362222184858401,
0.5));
#38103=CARTESIAN_POINT('',(-0.0970571419134453,0.362222184858401,0.475));
#38104=CARTESIAN_POINT('',(-0.11644947295219,0.382674169822262,0.45));
#38105=CARTESIAN_POINT('Ctrl Pts',(-0.0970571419134453,0.362222184858401,
0.475));
#38106=CARTESIAN_POINT('Ctrl Pts',(-0.106440527899932,0.372118306615104,
0.463012481414248));
#38107=CARTESIAN_POINT('Ctrl Pts',(-0.11644947295219,0.382674169822262,
0.45));
#38108=CARTESIAN_POINT('',(-0.0970571419134453,0.362222184858401,0.015));
#38109=CARTESIAN_POINT('',(-0.0970571419134453,0.362222184858401,0.5));
#38110=CARTESIAN_POINT('',(-0.11644947295219,0.382674169822262,0.04));
#38111=CARTESIAN_POINT('Ctrl Pts',(-0.11644947295219,0.382674169822262,
0.04));
#38112=CARTESIAN_POINT('Ctrl Pts',(-0.106440527899929,0.372118306615102,
0.0269875185857486));
#38113=CARTESIAN_POINT('Ctrl Pts',(-0.0970571419134453,0.362222184858401,
0.015));
#38114=CARTESIAN_POINT('',(-0.11644947295219,0.382674169822262,0.245));
#38115=CARTESIAN_POINT('Origin',(-0.0801836312165449,0.43263215932814,0.5));
#38116=CARTESIAN_POINT('',(-0.0904888830772255,0.389630288914294,0.45));
#38117=CARTESIAN_POINT('Ctrl Pts',(-0.0904888830772256,0.389630288914294,
0.45));
#38118=CARTESIAN_POINT('Ctrl Pts',(-0.0938789521539861,0.375484170691889,
0.463012481414251));
#38119=CARTESIAN_POINT('Ctrl Pts',(-0.0970571419134453,0.362222184858401,
0.475));
#38120=CARTESIAN_POINT('',(-0.0904888830772255,0.389630288914294,0.04));
#38121=CARTESIAN_POINT('',(-0.0904888830772255,0.389630288914294,0.245));
#38122=CARTESIAN_POINT('Ctrl Pts',(-0.0970571419134453,0.362222184858401,
0.015));
#38123=CARTESIAN_POINT('Ctrl Pts',(-0.093878952153988,0.375484170691881,
0.0269875185857416));
#38124=CARTESIAN_POINT('Ctrl Pts',(-0.0904888830772256,0.389630288914294,
0.04));
#38125=CARTESIAN_POINT('Origin',(0.0970571419134453,0.362222184858401,0.5));
#38126=CARTESIAN_POINT('',(0.0970571419134453,0.362222184858401,0.475));
#38127=CARTESIAN_POINT('',(0.0904888830772255,0.389630288914294,0.45));
#38128=CARTESIAN_POINT('Ctrl Pts',(0.0970571419134453,0.362222184858401,
0.475));
#38129=CARTESIAN_POINT('Ctrl Pts',(0.093878952153984,0.375484170691898,
0.463012481414244));
#38130=CARTESIAN_POINT('Ctrl Pts',(0.0904888830772255,0.389630288914294,
0.45));
#38131=CARTESIAN_POINT('',(0.0970571419134453,0.362222184858401,0.015));
#38132=CARTESIAN_POINT('',(0.0970571419134453,0.362222184858401,0.5));
#38133=CARTESIAN_POINT('',(0.0904888830772255,0.389630288914294,0.04));
#38134=CARTESIAN_POINT('Ctrl Pts',(0.0904888830772255,0.389630288914294,
0.04));
#38135=CARTESIAN_POINT('Ctrl Pts',(0.0938789521539869,0.375484170691886,
0.0269875185857455));
#38136=CARTESIAN_POINT('Ctrl Pts',(0.0970571419134453,0.362222184858401,
0.015));
#38137=CARTESIAN_POINT('',(0.0904888830772255,0.389630288914294,0.245));
#38138=CARTESIAN_POINT('Origin',(0.146875018062859,0.414762256080559,0.5));
#38139=CARTESIAN_POINT('',(0.11644947295219,0.382674169822262,0.45));
#38140=CARTESIAN_POINT('Ctrl Pts',(0.11644947295219,0.382674169822262,0.45));
#38141=CARTESIAN_POINT('Ctrl Pts',(0.106440527899934,0.372118306615107,
0.463012481414245));
#38142=CARTESIAN_POINT('Ctrl Pts',(0.0970571419134453,0.362222184858401,
0.475));
#38143=CARTESIAN_POINT('',(0.11644947295219,0.382674169822262,0.04));
#38144=CARTESIAN_POINT('',(0.11644947295219,0.382674169822262,0.245));
#38145=CARTESIAN_POINT('Ctrl Pts',(0.0970571419134453,0.362222184858401,
0.015));
#38146=CARTESIAN_POINT('Ctrl Pts',(0.106440527899938,0.372118306615111,
0.0269875185857598));
#38147=CARTESIAN_POINT('Ctrl Pts',(0.11644947295219,0.382674169822262,0.04));
#38148=CARTESIAN_POINT('Origin',(0.265165042944955,0.265165042944955,0.5));
#38149=CARTESIAN_POINT('',(0.265165042944955,0.265165042944955,0.475));
#38150=CARTESIAN_POINT('',(0.273180815962104,0.292185286745036,0.45));
#38151=CARTESIAN_POINT('Ctrl Pts',(0.265165042944955,0.265165042944955,
0.475));
#38152=CARTESIAN_POINT('Ctrl Pts',(0.269043642791962,0.27823935446112,0.463012481414247));
#38153=CARTESIAN_POINT('Ctrl Pts',(0.273180815962104,0.292185286745036,
0.45));
#38154=CARTESIAN_POINT('',(0.265165042944955,0.265165042944955,0.015));
#38155=CARTESIAN_POINT('',(0.265165042944955,0.265165042944955,0.5));
#38156=CARTESIAN_POINT('',(0.273180815962104,0.292185286745036,0.04));
#38157=CARTESIAN_POINT('Ctrl Pts',(0.273180815962104,0.292185286745036,
0.04));
#38158=CARTESIAN_POINT('Ctrl Pts',(0.26904364279196,0.278239354461114,0.0269875185857475));
#38159=CARTESIAN_POINT('Ctrl Pts',(0.265165042944955,0.265165042944955,
0.015));
#38160=CARTESIAN_POINT('',(0.273180815962104,0.292185286745036,0.245));
#38161=CARTESIAN_POINT('Origin',(0.334578624864014,0.285757141265281,0.5));
#38162=CARTESIAN_POINT('',(0.292185286745036,0.273180815962104,0.45));
#38163=CARTESIAN_POINT('Ctrl Pts',(0.292185286745036,0.273180815962104,
0.45));
#38164=CARTESIAN_POINT('Ctrl Pts',(0.278239354461118,0.269043642791961,
0.463012481414249));
#38165=CARTESIAN_POINT('Ctrl Pts',(0.265165042944955,0.265165042944955,
0.475));
#38166=CARTESIAN_POINT('',(0.292185286745036,0.273180815962104,0.04));
#38167=CARTESIAN_POINT('',(0.292185286745036,0.273180815962104,0.245));
#38168=CARTESIAN_POINT('Ctrl Pts',(0.265165042944955,0.265165042944955,
0.015));
#38169=CARTESIAN_POINT('Ctrl Pts',(0.278239354461114,0.26904364279196,0.0269875185857475));
#38170=CARTESIAN_POINT('Ctrl Pts',(0.292185286745036,0.273180815962104,
0.04));
#38171=CARTESIAN_POINT('Origin',(0.362222184858401,0.0970571419134453,0.5));
#38172=CARTESIAN_POINT('',(0.362222184858401,0.0970571419134453,0.475));
#38173=CARTESIAN_POINT('',(0.382674169822262,0.11644947295219,0.45));
#38174=CARTESIAN_POINT('Ctrl Pts',(0.362222184858401,0.0970571419134453,
0.475));
#38175=CARTESIAN_POINT('Ctrl Pts',(0.372118306615106,0.106440527899933,
0.463012481414246));
#38176=CARTESIAN_POINT('Ctrl Pts',(0.382674169822262,0.11644947295219,0.45));
#38177=CARTESIAN_POINT('',(0.362222184858401,0.0970571419134453,0.015));
#38178=CARTESIAN_POINT('',(0.362222184858401,0.0970571419134453,0.5));
#38179=CARTESIAN_POINT('',(0.382674169822262,0.11644947295219,0.04));
#38180=CARTESIAN_POINT('Ctrl Pts',(0.382674169822262,0.11644947295219,0.04));
#38181=CARTESIAN_POINT('Ctrl Pts',(0.372118306615112,0.106440527899938,
0.0269875185857607));
#38182=CARTESIAN_POINT('Ctrl Pts',(0.362222184858401,0.0970571419134453,
0.015));
#38183=CARTESIAN_POINT('',(0.382674169822262,0.11644947295219,0.245));
#38184=CARTESIAN_POINT('Origin',(0.43263215932814,0.0801836312165449,0.5));
#38185=CARTESIAN_POINT('',(0.389630288914294,0.0904888830772255,0.45));
#38186=CARTESIAN_POINT('Ctrl Pts',(0.389630288914294,0.0904888830772255,
0.45));
#38187=CARTESIAN_POINT('Ctrl Pts',(0.375484170691896,0.0938789521539845,
0.463012481414246));
#38188=CARTESIAN_POINT('Ctrl Pts',(0.362222184858401,0.0970571419134453,
0.475));
#38189=CARTESIAN_POINT('',(0.389630288914294,0.0904888830772255,0.04));
#38190=CARTESIAN_POINT('',(0.389630288914294,0.0904888830772255,0.245));
#38191=CARTESIAN_POINT('Ctrl Pts',(0.362222184858401,0.0970571419134453,
0.015));
#38192=CARTESIAN_POINT('Ctrl Pts',(0.375484170691883,0.0938789521539875,
0.0269875185857432));
#38193=CARTESIAN_POINT('Ctrl Pts',(0.389630288914294,0.0904888830772255,
0.04));
#38194=CARTESIAN_POINT('Origin',(0.324759526419165,0.1875,0.5));
#38195=CARTESIAN_POINT('',(0.324759526419165,0.1875,0.475));
#38196=CARTESIAN_POINT('',(0.339495522292874,0.211524916601068,0.45));
#38197=CARTESIAN_POINT('Ctrl Pts',(0.324759526419165,0.1875,0.475));
#38198=CARTESIAN_POINT('Ctrl Pts',(0.331889847003213,0.199124959645671,
0.463012481414251));
#38199=CARTESIAN_POINT('Ctrl Pts',(0.339495522292874,0.211524916601068,
0.45));
#38200=CARTESIAN_POINT('',(0.324759526419165,0.1875,0.015));
#38201=CARTESIAN_POINT('',(0.324759526419165,0.1875,0.5));
#38202=CARTESIAN_POINT('',(0.339495522292874,0.211524916601068,0.04));
#38203=CARTESIAN_POINT('Ctrl Pts',(0.339495522292874,0.211524916601068,
0.04));
#38204=CARTESIAN_POINT('Ctrl Pts',(0.331889847003218,0.199124959645679,
0.0269875185857566));
#38205=CARTESIAN_POINT('Ctrl Pts',(0.324759526419165,0.1875,0.015));
#38206=CARTESIAN_POINT('',(0.339495522292874,0.211524916601068,0.245));
#38207=CARTESIAN_POINT('Origin',(0.397137525113939,0.18942488259565,0.5));
#38208=CARTESIAN_POINT('',(0.352933712456347,0.188249288476161,0.45));
#38209=CARTESIAN_POINT('Ctrl Pts',(0.352933712456347,0.188249288476161,
0.45));
#38210=CARTESIAN_POINT('Ctrl Pts',(0.338392197082318,0.187862558940078,
0.463012481414243));
#38211=CARTESIAN_POINT('Ctrl Pts',(0.324759526419165,0.1875,0.475));
#38212=CARTESIAN_POINT('',(0.352933712456347,0.188249288476161,0.04));
#38213=CARTESIAN_POINT('',(0.352933712456347,0.188249288476161,0.245));
#38214=CARTESIAN_POINT('Ctrl Pts',(0.324759526419165,0.1875,0.015));
#38215=CARTESIAN_POINT('Ctrl Pts',(0.338392197082309,0.187862558940078,
0.0269875185857488));
#38216=CARTESIAN_POINT('Ctrl Pts',(0.352933712456347,0.188249288476161,
0.04));
#38217=CARTESIAN_POINT('Origin',(0.1875,0.324759526419164,0.5));
#38218=CARTESIAN_POINT('',(0.1875,0.324759526419164,0.475));
#38219=CARTESIAN_POINT('',(0.188249288476161,0.352933712456347,0.45));
#38220=CARTESIAN_POINT('Ctrl Pts',(0.1875,0.324759526419164,0.475));
#38221=CARTESIAN_POINT('Ctrl Pts',(0.187862558940078,0.338392197082313,
0.463012481414248));
#38222=CARTESIAN_POINT('Ctrl Pts',(0.188249288476161,0.352933712456347,
0.45));
#38223=CARTESIAN_POINT('',(0.1875,0.324759526419164,0.0150000000000001));
#38224=CARTESIAN_POINT('',(0.1875,0.324759526419164,0.5));
#38225=CARTESIAN_POINT('',(0.188249288476161,0.352933712456347,0.04));
#38226=CARTESIAN_POINT('Ctrl Pts',(0.188249288476161,0.352933712456347,
0.04));
#38227=CARTESIAN_POINT('Ctrl Pts',(0.187862558940078,0.338392197082318,
0.0269875185857566));
#38228=CARTESIAN_POINT('Ctrl Pts',(0.1875,0.324759526419164,0.0150000000000001));
#38229=CARTESIAN_POINT('',(0.188249288476161,0.352933712456347,0.245));
#38230=CARTESIAN_POINT('Origin',(0.249218744246926,0.362615522993687,0.5));
#38231=CARTESIAN_POINT('',(0.211524916601068,0.339495522292874,0.45));
#38232=CARTESIAN_POINT('Ctrl Pts',(0.211524916601068,0.339495522292874,
0.45));
#38233=CARTESIAN_POINT('Ctrl Pts',(0.199124959645677,0.331889847003217,
0.463012481414245));
#38234=CARTESIAN_POINT('Ctrl Pts',(0.1875,0.324759526419164,0.475));
#38235=CARTESIAN_POINT('',(0.211524916601068,0.339495522292874,0.04));
#38236=CARTESIAN_POINT('',(0.211524916601068,0.339495522292874,0.245));
#38237=CARTESIAN_POINT('Ctrl Pts',(0.1875,0.324759526419164,0.015));
#38238=CARTESIAN_POINT('Ctrl Pts',(0.199124959645668,0.331889847003211,
0.0269875185857458));
#38239=CARTESIAN_POINT('Ctrl Pts',(0.211524916601068,0.339495522292874,
0.04));
#38240=CARTESIAN_POINT('Origin',(2.29621274840129E-17,0.375,0.5));
#38241=CARTESIAN_POINT('',(2.29621274840129E-17,0.375,0.475));
#38242=CARTESIAN_POINT('',(-0.0134381901634729,0.399774205077229,0.45));
#38243=CARTESIAN_POINT('Ctrl Pts',(2.29621274840129E-17,0.375,0.475));
#38244=CARTESIAN_POINT('Ctrl Pts',(-0.00650235007909964,0.386987518585756,
0.463012481414244));
#38245=CARTESIAN_POINT('Ctrl Pts',(-0.0134381901634728,0.399774205077229,
0.45));
#38246=CARTESIAN_POINT('',(2.29621274840129E-17,0.375,0.015));
#38247=CARTESIAN_POINT('',(2.29621274840129E-17,0.375,0.5));
#38248=CARTESIAN_POINT('',(-0.0134381901634729,0.399774205077229,0.04));
#38249=CARTESIAN_POINT('Ctrl Pts',(-0.0134381901634729,0.399774205077229,
0.04));
#38250=CARTESIAN_POINT('Ctrl Pts',(-0.00650235007909639,0.38698751858575,
0.0269875185857497));
#38251=CARTESIAN_POINT('Ctrl Pts',(2.29621274840129E-17,0.375,0.015));
#38252=CARTESIAN_POINT('',(-0.0134381901634729,0.399774205077229,0.245));
#38253=CARTESIAN_POINT('Origin',(0.0345220021202518,0.438643626842576,0.5));
#38254=CARTESIAN_POINT('',(0.013438190163473,0.399774205077229,0.45));
#38255=CARTESIAN_POINT('Ctrl Pts',(0.013438190163473,0.399774205077229,
0.45));
#38256=CARTESIAN_POINT('Ctrl Pts',(0.00650235007909615,0.386987518585749,
0.463012481414251));
#38257=CARTESIAN_POINT('Ctrl Pts',(2.29621274840129E-17,0.375,0.475));
#38258=CARTESIAN_POINT('',(0.013438190163473,0.399774205077229,0.04));
#38259=CARTESIAN_POINT('',(0.013438190163473,0.399774205077229,0.245));
#38260=CARTESIAN_POINT('Ctrl Pts',(2.29621274840129E-17,0.375,0.015));
#38261=CARTESIAN_POINT('Ctrl Pts',(0.00650235007909749,0.386987518585752,
0.0269875185857516));
#38262=CARTESIAN_POINT('Ctrl Pts',(0.013438190163473,0.399774205077229,
0.04));
#38263=CARTESIAN_POINT('Origin',(-0.1875,0.324759526419165,0.5));
#38264=CARTESIAN_POINT('',(-0.1875,0.324759526419165,0.475));
#38265=CARTESIAN_POINT('',(-0.211524916601068,0.339495522292874,0.45));
#38266=CARTESIAN_POINT('Ctrl Pts',(-0.1875,0.324759526419165,0.475));
#38267=CARTESIAN_POINT('Ctrl Pts',(-0.199124959645671,0.331889847003213,
0.463012481414252));
#38268=CARTESIAN_POINT('Ctrl Pts',(-0.211524916601068,0.339495522292874,
0.45));
#38269=CARTESIAN_POINT('',(-0.1875,0.324759526419165,0.015));
#38270=CARTESIAN_POINT('',(-0.1875,0.324759526419165,0.5));
#38271=CARTESIAN_POINT('',(-0.211524916601068,0.339495522292874,0.04));
#38272=CARTESIAN_POINT('Ctrl Pts',(-0.211524916601068,0.339495522292874,
0.04));
#38273=CARTESIAN_POINT('Ctrl Pts',(-0.199124959645683,0.33188984700322,
0.0269875185857606));
#38274=CARTESIAN_POINT('Ctrl Pts',(-0.1875,0.324759526419165,0.015));
#38275=CARTESIAN_POINT('',(-0.211524916601068,0.339495522292874,0.245));
#38276=CARTESIAN_POINT('Origin',(-0.18942488259565,0.397137525113939,0.5));
#38277=CARTESIAN_POINT('',(-0.188249288476161,0.352933712456347,0.45));
#38278=CARTESIAN_POINT('Ctrl Pts',(-0.188249288476161,0.352933712456347,
0.45));
#38279=CARTESIAN_POINT('Ctrl Pts',(-0.187862558940078,0.33839219708231,
0.46301248141425));
#38280=CARTESIAN_POINT('Ctrl Pts',(-0.1875,0.324759526419165,0.475));
#38281=CARTESIAN_POINT('',(-0.188249288476161,0.352933712456347,0.04));
#38282=CARTESIAN_POINT('',(-0.188249288476161,0.352933712456347,0.245));
#38283=CARTESIAN_POINT('Ctrl Pts',(-0.1875,0.324759526419165,0.015));
#38284=CARTESIAN_POINT('Ctrl Pts',(-0.187862558940077,0.338392197082308,
0.0269875185857478));
#38285=CARTESIAN_POINT('Ctrl Pts',(-0.188249288476161,0.352933712456347,
0.04));
#38286=CARTESIAN_POINT('Origin',(-0.324759526419165,0.1875,0.5));
#38287=CARTESIAN_POINT('',(-0.324759526419165,0.1875,0.475));
#38288=CARTESIAN_POINT('',(-0.352933712456347,0.188249288476161,0.45));
#38289=CARTESIAN_POINT('Ctrl Pts',(-0.324759526419165,0.1875,0.475));
#38290=CARTESIAN_POINT('Ctrl Pts',(-0.338392197082309,0.187862558940077,
0.463012481414251));
#38291=CARTESIAN_POINT('Ctrl Pts',(-0.352933712456347,0.188249288476161,
0.45));
#38292=CARTESIAN_POINT('',(-0.324759526419165,0.1875,0.015));
#38293=CARTESIAN_POINT('',(-0.324759526419165,0.1875,0.5));
#38294=CARTESIAN_POINT('',(-0.352933712456347,0.188249288476161,0.04));
#38295=CARTESIAN_POINT('Ctrl Pts',(-0.352933712456347,0.188249288476161,
0.04));
#38296=CARTESIAN_POINT('Ctrl Pts',(-0.338392197082316,0.187862558940078,
0.0269875185857554));
#38297=CARTESIAN_POINT('Ctrl Pts',(-0.324759526419165,0.1875,0.015));
#38298=CARTESIAN_POINT('',(-0.352933712456347,0.188249288476161,0.245));
#38299=CARTESIAN_POINT('Origin',(-0.362615522993687,0.249218744246926,0.5));
#38300=CARTESIAN_POINT('',(-0.339495522292874,0.211524916601068,0.45));
#38301=CARTESIAN_POINT('Ctrl Pts',(-0.339495522292874,0.211524916601068,
0.45));
#38302=CARTESIAN_POINT('Ctrl Pts',(-0.331889847003215,0.199124959645674,
0.463012481414249));
#38303=CARTESIAN_POINT('Ctrl Pts',(-0.324759526419165,0.1875,0.475));
#38304=CARTESIAN_POINT('',(-0.339495522292874,0.211524916601068,0.04));
#38305=CARTESIAN_POINT('',(-0.339495522292874,0.211524916601068,0.245));
#38306=CARTESIAN_POINT('Ctrl Pts',(-0.324759526419164,0.1875,0.015));
#38307=CARTESIAN_POINT('Ctrl Pts',(-0.331889847003215,0.199124959645674,
0.0269875185857514));
#38308=CARTESIAN_POINT('Ctrl Pts',(-0.339495522292874,0.211524916601068,
0.04));
#38309=CARTESIAN_POINT('Origin',(0.375,0.,0.5));
#38310=CARTESIAN_POINT('',(0.375,0.,0.475));
#38311=CARTESIAN_POINT('',(0.399774205077229,0.013438190163473,0.45));
#38312=CARTESIAN_POINT('Ctrl Pts',(0.375,0.,0.475));
#38313=CARTESIAN_POINT('Ctrl Pts',(0.386987518585754,0.00650235007909865,
0.463012481414246));
#38314=CARTESIAN_POINT('Ctrl Pts',(0.399774205077229,0.0134381901634729,
0.45));
#38315=CARTESIAN_POINT('',(0.375,0.,0.015));
#38316=CARTESIAN_POINT('',(0.375,0.,0.5));
#38317=CARTESIAN_POINT('',(0.399774205077229,0.013438190163473,0.04));
#38318=CARTESIAN_POINT('Ctrl Pts',(0.399774205077229,0.0134381901634729,
0.04));
#38319=CARTESIAN_POINT('Ctrl Pts',(0.38698751858575,0.00650235007909652,
0.02698751858575));
#38320=CARTESIAN_POINT('Ctrl Pts',(0.375,0.,0.015));
#38321=CARTESIAN_POINT('',(0.399774205077229,0.013438190163473,0.245));
#38322=CARTESIAN_POINT('Origin',(0.438643626842576,-0.0345220021202518,
0.5));
#38323=CARTESIAN_POINT('',(0.399774205077229,-0.013438190163473,0.45));
#38324=CARTESIAN_POINT('Ctrl Pts',(0.399774205077229,-0.0134381901634729,
0.45));
#38325=CARTESIAN_POINT('Ctrl Pts',(0.386987518585751,-0.00650235007909692,
0.463012481414249));
#38326=CARTESIAN_POINT('Ctrl Pts',(0.375,0.,0.475));
#38327=CARTESIAN_POINT('',(0.399774205077229,-0.013438190163473,0.04));
#38328=CARTESIAN_POINT('',(0.399774205077229,-0.013438190163473,0.245));
#38329=CARTESIAN_POINT('Ctrl Pts',(0.375,0.,0.015));
#38330=CARTESIAN_POINT('Ctrl Pts',(0.386987518585746,-0.00650235007909417,
0.0269875185857456));
#38331=CARTESIAN_POINT('Ctrl Pts',(0.399774205077229,-0.0134381901634729,
0.04));
#38332=CARTESIAN_POINT('Origin',(-0.362222184858401,-0.0970571419134453,
0.5));
#38333=CARTESIAN_POINT('',(-0.362222184858401,-0.0970571419134453,0.475));
#38334=CARTESIAN_POINT('',(-0.382674169822262,-0.11644947295219,0.45));
#38335=CARTESIAN_POINT('Ctrl Pts',(-0.362222184858401,-0.0970571419134453,
0.475));
#38336=CARTESIAN_POINT('Ctrl Pts',(-0.372118306615105,-0.106440527899932,
0.463012481414247));
#38337=CARTESIAN_POINT('Ctrl Pts',(-0.382674169822262,-0.11644947295219,
0.45));
#38338=CARTESIAN_POINT('',(-0.362222184858401,-0.0970571419134453,0.015));
#38339=CARTESIAN_POINT('',(-0.362222184858401,-0.0970571419134453,0.5));
#38340=CARTESIAN_POINT('',(-0.382674169822262,-0.11644947295219,0.04));
#38341=CARTESIAN_POINT('Ctrl Pts',(-0.382674169822262,-0.11644947295219,
0.04));
#38342=CARTESIAN_POINT('Ctrl Pts',(-0.372118306615101,-0.106440527899928,
0.0269875185857478));
#38343=CARTESIAN_POINT('Ctrl Pts',(-0.362222184858401,-0.0970571419134453,
0.015));
#38344=CARTESIAN_POINT('',(-0.382674169822262,-0.11644947295219,0.245));
#38345=CARTESIAN_POINT('Origin',(-0.43263215932814,-0.0801836312165449,
0.5));
#38346=CARTESIAN_POINT('',(-0.389630288914294,-0.0904888830772255,0.45));
#38347=CARTESIAN_POINT('Ctrl Pts',(-0.389630288914294,-0.0904888830772256,
0.45));
#38348=CARTESIAN_POINT('Ctrl Pts',(-0.375484170691889,-0.093878952153986,
0.463012481414251));
#38349=CARTESIAN_POINT('Ctrl Pts',(-0.362222184858401,-0.0970571419134453,
0.475));
#38350=CARTESIAN_POINT('',(-0.389630288914294,-0.0904888830772255,0.04));
#38351=CARTESIAN_POINT('',(-0.389630288914294,-0.0904888830772255,0.245));
#38352=CARTESIAN_POINT('Ctrl Pts',(-0.362222184858401,-0.0970571419134453,
0.015));
#38353=CARTESIAN_POINT('Ctrl Pts',(-0.375484170691881,-0.0938789521539879,
0.0269875185857416));
#38354=CARTESIAN_POINT('Ctrl Pts',(-0.389630288914294,-0.0904888830772256,
0.04));
#38355=CARTESIAN_POINT('Origin',(-0.265165042944955,-0.265165042944955,
0.5));
#38356=CARTESIAN_POINT('',(-0.265165042944955,-0.265165042944955,0.475));
#38357=CARTESIAN_POINT('',(-0.273180815962104,-0.292185286745036,0.45));
#38358=CARTESIAN_POINT('Ctrl Pts',(-0.265165042944955,-0.265165042944955,
0.475));
#38359=CARTESIAN_POINT('Ctrl Pts',(-0.269043642791962,-0.278239354461122,
0.463012481414245));
#38360=CARTESIAN_POINT('Ctrl Pts',(-0.273180815962104,-0.292185286745036,
0.45));
#38361=CARTESIAN_POINT('',(-0.265165042944955,-0.265165042944955,0.015));
#38362=CARTESIAN_POINT('',(-0.265165042944955,-0.265165042944955,0.5));
#38363=CARTESIAN_POINT('',(-0.273180815962104,-0.292185286745036,0.04));
#38364=CARTESIAN_POINT('Ctrl Pts',(-0.273180815962104,-0.292185286745036,
0.04));
#38365=CARTESIAN_POINT('Ctrl Pts',(-0.269043642791963,-0.278239354461123,
0.0269875185857556));
#38366=CARTESIAN_POINT('Ctrl Pts',(-0.265165042944955,-0.265165042944955,
0.015));
#38367=CARTESIAN_POINT('',(-0.273180815962104,-0.292185286745036,0.245));
#38368=CARTESIAN_POINT('Origin',(-0.334578624864014,-0.285757141265281,
0.5));
#38369=CARTESIAN_POINT('',(-0.292185286745036,-0.273180815962104,0.45));
#38370=CARTESIAN_POINT('Ctrl Pts',(-0.292185286745036,-0.273180815962104,
0.45));
#38371=CARTESIAN_POINT('Ctrl Pts',(-0.278239354461122,-0.269043642791962,
0.463012481414245));
#38372=CARTESIAN_POINT('Ctrl Pts',(-0.265165042944955,-0.265165042944955,
0.475));
#38373=CARTESIAN_POINT('',(-0.292185286745036,-0.273180815962104,0.04));
#38374=CARTESIAN_POINT('',(-0.292185286745036,-0.273180815962104,0.245));
#38375=CARTESIAN_POINT('Ctrl Pts',(-0.265165042944955,-0.265165042944955,
0.015));
#38376=CARTESIAN_POINT('Ctrl Pts',(-0.278239354461126,-0.269043642791964,
0.0269875185857586));
#38377=CARTESIAN_POINT('Ctrl Pts',(-0.292185286745036,-0.273180815962104,
0.04));
#38378=CARTESIAN_POINT('Origin',(-0.0970571419134452,-0.362222184858401,
0.5));
#38379=CARTESIAN_POINT('',(-0.0970571419134452,-0.362222184858401,0.475));
#38380=CARTESIAN_POINT('',(-0.0904888830772255,-0.389630288914294,0.45));
#38381=CARTESIAN_POINT('Ctrl Pts',(-0.0970571419134452,-0.362222184858401,
0.475));
#38382=CARTESIAN_POINT('Ctrl Pts',(-0.0938789521539842,-0.375484170691897,
0.463012481414244));
#38383=CARTESIAN_POINT('Ctrl Pts',(-0.0904888830772255,-0.389630288914294,
0.45));
#38384=CARTESIAN_POINT('',(-0.0970571419134452,-0.362222184858401,0.015));
#38385=CARTESIAN_POINT('',(-0.0970571419134452,-0.362222184858401,0.5));
#38386=CARTESIAN_POINT('',(-0.0904888830772255,-0.389630288914294,0.04));
#38387=CARTESIAN_POINT('Ctrl Pts',(-0.0904888830772256,-0.389630288914294,
0.04));
#38388=CARTESIAN_POINT('Ctrl Pts',(-0.0938789521539856,-0.375484170691891,
0.0269875185857502));
#38389=CARTESIAN_POINT('Ctrl Pts',(-0.0970571419134452,-0.362222184858401,
0.015));
#38390=CARTESIAN_POINT('',(-0.0904888830772255,-0.389630288914294,0.245));
#38391=CARTESIAN_POINT('Origin',(-0.146875018062859,-0.414762256080559,
0.5));
#38392=CARTESIAN_POINT('',(-0.11644947295219,-0.382674169822262,0.45));
#38393=CARTESIAN_POINT('Ctrl Pts',(-0.11644947295219,-0.382674169822262,
0.45));
#38394=CARTESIAN_POINT('Ctrl Pts',(-0.106440527899936,-0.372118306615109,
0.463012481414242));
#38395=CARTESIAN_POINT('Ctrl Pts',(-0.0970571419134452,-0.362222184858401,
0.475));
#38396=CARTESIAN_POINT('',(-0.11644947295219,-0.382674169822262,0.04));
#38397=CARTESIAN_POINT('',(-0.11644947295219,-0.382674169822262,0.245));
#38398=CARTESIAN_POINT('Ctrl Pts',(-0.0970571419134452,-0.362222184858401,
0.015));
#38399=CARTESIAN_POINT('Ctrl Pts',(-0.106440527899943,-0.372118306615116,
0.0269875185857666));
#38400=CARTESIAN_POINT('Ctrl Pts',(-0.11644947295219,-0.382674169822262,
0.04));
#38401=CARTESIAN_POINT('Origin',(0.0970571419134451,-0.362222184858401,
0.5));
#38402=CARTESIAN_POINT('',(0.0970571419134451,-0.362222184858401,0.475));
#38403=CARTESIAN_POINT('',(0.11644947295219,-0.382674169822262,0.45));
#38404=CARTESIAN_POINT('Ctrl Pts',(0.0970571419134451,-0.362222184858401,
0.475));
#38405=CARTESIAN_POINT('Ctrl Pts',(0.106440527899935,-0.372118306615108,
0.463012481414243));
#38406=CARTESIAN_POINT('Ctrl Pts',(0.11644947295219,-0.382674169822262,
0.45));
#38407=CARTESIAN_POINT('',(0.0970571419134451,-0.362222184858401,0.0150000000000001));
#38408=CARTESIAN_POINT('',(0.0970571419134451,-0.362222184858401,0.5));
#38409=CARTESIAN_POINT('',(0.11644947295219,-0.382674169822262,0.04));
#38410=CARTESIAN_POINT('Ctrl Pts',(0.11644947295219,-0.382674169822262,
0.04));
#38411=CARTESIAN_POINT('Ctrl Pts',(0.106440527899933,-0.372118306615106,
0.0269875185857537));
#38412=CARTESIAN_POINT('Ctrl Pts',(0.0970571419134451,-0.362222184858401,
0.0150000000000001));
#38413=CARTESIAN_POINT('',(0.11644947295219,-0.382674169822262,0.245));
#38414=CARTESIAN_POINT('Origin',(0.0801836312165449,-0.43263215932814,0.5));
#38415=CARTESIAN_POINT('',(0.0904888830772254,-0.389630288914294,0.45));
#38416=CARTESIAN_POINT('Ctrl Pts',(0.0904888830772254,-0.389630288914294,
0.45));
#38417=CARTESIAN_POINT('Ctrl Pts',(0.0938789521539843,-0.375484170691896,
0.463012481414245));
#38418=CARTESIAN_POINT('Ctrl Pts',(0.0970571419134451,-0.362222184858401,
0.475));
#38419=CARTESIAN_POINT('',(0.0904888830772254,-0.389630288914294,0.04));
#38420=CARTESIAN_POINT('',(0.0904888830772254,-0.389630288914294,0.245));
#38421=CARTESIAN_POINT('Ctrl Pts',(0.0970571419134451,-0.362222184858401,
0.0150000000000001));
#38422=CARTESIAN_POINT('Ctrl Pts',(0.0938789521539861,-0.375484170691888,
0.0269875185857479));
#38423=CARTESIAN_POINT('Ctrl Pts',(0.0904888830772254,-0.389630288914294,
0.04));
#38424=CARTESIAN_POINT('Origin',(0.265165042944955,-0.265165042944955,0.5));
#38425=CARTESIAN_POINT('',(0.265165042944955,-0.265165042944955,0.475));
#38426=CARTESIAN_POINT('',(0.292185286745036,-0.273180815962104,0.45));
#38427=CARTESIAN_POINT('Ctrl Pts',(0.265165042944955,-0.265165042944955,
0.475));
#38428=CARTESIAN_POINT('Ctrl Pts',(0.278239354461118,-0.269043642791961,
0.463012481414249));
#38429=CARTESIAN_POINT('Ctrl Pts',(0.292185286745036,-0.273180815962104,
0.45));
#38430=CARTESIAN_POINT('',(0.265165042944955,-0.265165042944955,0.015));
#38431=CARTESIAN_POINT('',(0.265165042944955,-0.265165042944955,0.5));
#38432=CARTESIAN_POINT('',(0.292185286745036,-0.273180815962104,0.04));
#38433=CARTESIAN_POINT('Ctrl Pts',(0.292185286745036,-0.273180815962104,
0.04));
#38434=CARTESIAN_POINT('Ctrl Pts',(0.278239354461123,-0.269043642791963,
0.0269875185857557));
#38435=CARTESIAN_POINT('Ctrl Pts',(0.265165042944955,-0.265165042944955,
0.015));
#38436=CARTESIAN_POINT('',(0.292185286745036,-0.273180815962104,0.245));
#38437=CARTESIAN_POINT('Origin',(0.285757141265281,-0.334578624864014,0.5));
#38438=CARTESIAN_POINT('',(0.273180815962104,-0.292185286745036,0.45));
#38439=CARTESIAN_POINT('Ctrl Pts',(0.273180815962104,-0.292185286745036,
0.45));
#38440=CARTESIAN_POINT('Ctrl Pts',(0.269043642791963,-0.278239354461126,
0.463012481414242));
#38441=CARTESIAN_POINT('Ctrl Pts',(0.265165042944955,-0.265165042944955,
0.475));
#38442=CARTESIAN_POINT('',(0.273180815962104,-0.292185286745036,0.04));
#38443=CARTESIAN_POINT('',(0.273180815962104,-0.292185286745036,0.245));
#38444=CARTESIAN_POINT('Ctrl Pts',(0.265165042944955,-0.265165042944955,
0.015));
#38445=CARTESIAN_POINT('Ctrl Pts',(0.269043642791962,-0.278239354461121,
0.0269875185857534));
#38446=CARTESIAN_POINT('Ctrl Pts',(0.273180815962104,-0.292185286745036,
0.04));
#38447=CARTESIAN_POINT('Origin',(0.362222184858401,-0.0970571419134452,
0.5));
#38448=CARTESIAN_POINT('',(0.362222184858401,-0.0970571419134452,0.475));
#38449=CARTESIAN_POINT('',(0.389630288914294,-0.0904888830772255,0.45));
#38450=CARTESIAN_POINT('Ctrl Pts',(0.362222184858401,-0.0970571419134452,
0.475));
#38451=CARTESIAN_POINT('Ctrl Pts',(0.375484170691892,-0.0938789521539854,
0.463012481414249));
#38452=CARTESIAN_POINT('Ctrl Pts',(0.389630288914294,-0.0904888830772255,
0.45));
#38453=CARTESIAN_POINT('',(0.362222184858401,-0.0970571419134452,0.015));
#38454=CARTESIAN_POINT('',(0.362222184858401,-0.0970571419134452,0.5));
#38455=CARTESIAN_POINT('',(0.389630288914294,-0.0904888830772255,0.04));
#38456=CARTESIAN_POINT('Ctrl Pts',(0.389630288914294,-0.0904888830772256,
0.04));
#38457=CARTESIAN_POINT('Ctrl Pts',(0.375484170691905,-0.0938789521539823,
0.0269875185857627));
#38458=CARTESIAN_POINT('Ctrl Pts',(0.362222184858401,-0.0970571419134452,
0.015));
#38459=CARTESIAN_POINT('',(0.389630288914294,-0.0904888830772255,0.245));
#38460=CARTESIAN_POINT('Origin',(0.414762256080559,-0.146875018062859,0.5));
#38461=CARTESIAN_POINT('',(0.382674169822262,-0.11644947295219,0.45));
#38462=CARTESIAN_POINT('Ctrl Pts',(0.382674169822262,-0.11644947295219,
0.45));
#38463=CARTESIAN_POINT('Ctrl Pts',(0.372118306615106,-0.106440527899933,
0.463012481414245));
#38464=CARTESIAN_POINT('Ctrl Pts',(0.362222184858401,-0.0970571419134452,
0.475));
#38465=CARTESIAN_POINT('',(0.382674169822262,-0.11644947295219,0.04));
#38466=CARTESIAN_POINT('',(0.382674169822262,-0.11644947295219,0.245));
#38467=CARTESIAN_POINT('Ctrl Pts',(0.362222184858401,-0.0970571419134452,
0.015));
#38468=CARTESIAN_POINT('Ctrl Pts',(0.372118306615097,-0.106440527899925,
0.0269875185857436));
#38469=CARTESIAN_POINT('Ctrl Pts',(0.382674169822262,-0.11644947295219,
0.04));
#38470=CARTESIAN_POINT('Origin',(0.,0.,0.245));
#38471=CARTESIAN_POINT('Origin',(0.,0.,0.45));
#38472=CARTESIAN_POINT('Origin',(0.,0.,0.04));
#38473=CARTESIAN_POINT('Origin',(0.,0.,0.245));
#38474=CARTESIAN_POINT('Origin',(0.,0.,0.45));
#38475=CARTESIAN_POINT('Origin',(0.,0.,0.04));
#38476=CARTESIAN_POINT('Origin',(0.,0.,0.245));
#38477=CARTESIAN_POINT('Origin',(0.,0.,0.04));
#38478=CARTESIAN_POINT('Origin',(0.,0.,0.45));
#38479=CARTESIAN_POINT('Origin',(0.,0.,0.245));
#38480=CARTESIAN_POINT('Origin',(0.,0.,0.45));
#38481=CARTESIAN_POINT('Origin',(0.,0.,0.04));
#38482=CARTESIAN_POINT('Origin',(0.,0.,0.245));
#38483=CARTESIAN_POINT('Origin',(0.,0.,0.04));
#38484=CARTESIAN_POINT('Origin',(0.,0.,0.45));
#38485=CARTESIAN_POINT('Origin',(0.,0.,0.245));
#38486=CARTESIAN_POINT('Origin',(0.,0.,0.45));
#38487=CARTESIAN_POINT('Origin',(0.,0.,0.04));
#38488=CARTESIAN_POINT('Origin',(0.,0.,0.245));
#38489=CARTESIAN_POINT('Origin',(0.,0.,0.04));
#38490=CARTESIAN_POINT('Origin',(0.,0.,0.45));
#38491=CARTESIAN_POINT('Origin',(0.,0.,0.245));
#38492=CARTESIAN_POINT('Origin',(0.,0.,0.45));
#38493=CARTESIAN_POINT('Origin',(0.,0.,0.04));
#38494=CARTESIAN_POINT('Origin',(0.,0.,0.245));
#38495=CARTESIAN_POINT('Origin',(0.,0.,0.04));
#38496=CARTESIAN_POINT('Origin',(0.,0.,0.45));
#38497=CARTESIAN_POINT('Origin',(0.,0.,0.245));
#38498=CARTESIAN_POINT('Origin',(0.,0.,0.45));
#38499=CARTESIAN_POINT('Origin',(0.,0.,0.04));
#38500=CARTESIAN_POINT('Origin',(0.,0.,0.245));
#38501=CARTESIAN_POINT('Origin',(0.,0.,0.04));
#38502=CARTESIAN_POINT('Origin',(0.,0.,0.45));
#38503=CARTESIAN_POINT('Origin',(0.,0.,0.245));
#38504=CARTESIAN_POINT('Origin',(0.,0.,0.45));
#38505=CARTESIAN_POINT('Origin',(0.,0.,0.04));
#38506=CARTESIAN_POINT('Origin',(0.,0.,0.245));
#38507=CARTESIAN_POINT('Origin',(0.,0.,0.45));
#38508=CARTESIAN_POINT('Origin',(0.,0.,0.04));
#38509=CARTESIAN_POINT('Origin',(0.,0.,0.245));
#38510=CARTESIAN_POINT('Origin',(0.,0.,0.04));
#38511=CARTESIAN_POINT('Origin',(0.,0.,0.45));
#38512=CARTESIAN_POINT('Origin',(0.,0.,0.245));
#38513=CARTESIAN_POINT('Origin',(0.,0.,0.45));
#38514=CARTESIAN_POINT('Origin',(0.,0.,0.04));
#38515=CARTESIAN_POINT('Origin',(0.,0.,0.245));
#38516=CARTESIAN_POINT('Origin',(0.,0.,0.04));
#38517=CARTESIAN_POINT('Origin',(0.,0.,0.45));
#38518=CARTESIAN_POINT('Origin',(0.,0.,0.245));
#38519=CARTESIAN_POINT('Origin',(0.,0.,0.45));
#38520=CARTESIAN_POINT('Origin',(0.,0.,0.04));
#38521=CARTESIAN_POINT('Origin',(0.,0.,0.245));
#38522=CARTESIAN_POINT('Origin',(0.,0.,0.04));
#38523=CARTESIAN_POINT('Origin',(0.,0.,0.45));
#38524=CARTESIAN_POINT('Origin',(0.,0.,0.245));
#38525=CARTESIAN_POINT('Origin',(0.,0.,0.45));
#38526=CARTESIAN_POINT('Origin',(0.,0.,0.04));
#38527=CARTESIAN_POINT('Origin',(0.,0.,0.245));
#38528=CARTESIAN_POINT('Origin',(0.,0.,0.04));
#38529=CARTESIAN_POINT('Origin',(0.,0.,0.45));
#38530=CARTESIAN_POINT('Origin',(0.,0.,0.245));
#38531=CARTESIAN_POINT('Origin',(0.,0.,0.45));
#38532=CARTESIAN_POINT('Origin',(0.,0.,0.04));
#38533=CARTESIAN_POINT('Origin',(0.,0.,0.245));
#38534=CARTESIAN_POINT('Origin',(0.,0.,0.04));
#38535=CARTESIAN_POINT('Origin',(0.,0.,0.45));
#38536=CARTESIAN_POINT('Origin',(0.,0.,0.245));
#38537=CARTESIAN_POINT('Origin',(0.,0.,0.45));
#38538=CARTESIAN_POINT('Origin',(0.,0.,0.04));
#38539=CARTESIAN_POINT('Origin',(0.,0.,0.245));
#38540=CARTESIAN_POINT('Origin',(0.,0.,0.04));
#38541=CARTESIAN_POINT('Origin',(0.,0.,0.45));
#38542=CARTESIAN_POINT('Origin',(0.,0.,0.02));
#38543=CARTESIAN_POINT('',(-0.36,-4.40872847693047E-17,1.04083408558608E-17));
#38544=CARTESIAN_POINT('',(-0.38,-4.65365783675994E-17,0.02));
#38545=CARTESIAN_POINT('Origin',(0.,0.,0.));
#38546=CARTESIAN_POINT('Origin',(0.17,0.,-0.8));
#38547=CARTESIAN_POINT('',(-0.17,-2.0818995585505E-17,-0.8));
#38548=CARTESIAN_POINT('Origin',(0.,0.,-0.8));
#38549=CARTESIAN_POINT('Origin',(0.,0.,-0.785));
#38550=CARTESIAN_POINT('',(-0.185,-2.2655965784226E-17,-0.785));
#38551=CARTESIAN_POINT('Origin',(0.,0.,-0.385));
#38552=CARTESIAN_POINT('Origin',(0.,0.,0.));
#38553=CARTESIAN_POINT('Origin',(0.36,0.,0.));
#38554=CARTESIAN_POINT('Origin',(0.,0.,0.475));
#38555=CARTESIAN_POINT('',(-0.35,-4.28626379701574E-17,0.5));
#38556=CARTESIAN_POINT('Origin',(0.,0.,0.5));
#38557=CARTESIAN_POINT('',(-0.375,-4.59242549680257E-17,0.475));
#38558=CARTESIAN_POINT('Origin',(0.,0.,0.5));
#38559=CARTESIAN_POINT('',(0.,0.,0.));
#38560=CARTESIAN_POINT('',(0.,0.,0.));
#38561=CARTESIAN_POINT('',(0.,0.,0.));
#38562=CARTESIAN_POINT('',(0.,0.,0.));
#38563=CARTESIAN_POINT('',(0.,0.,0.));
#38564=CARTESIAN_POINT('',(0.,0.,0.));
#38565=CARTESIAN_POINT('',(2.,-1.03213203435478,7.3));
#38566=CARTESIAN_POINT('',(2.,0.167867965645222,7.3));
#38567=CARTESIAN_POINT('',(1.7,-0.25,10.));
#38568=CARTESIAN_POINT('',(1.7,-0.65,10.));
#38569=CARTESIAN_POINT('',(0.,-1.51,3.4));
#38570=CARTESIAN_POINT('',(0.,1.51,1.4));
#38571=CARTESIAN_POINT('',(0.,1.11,5.2));
#38572=CARTESIAN_POINT('',(0.,0.,0.));
#38573=CARTESIAN_POINT('',(2.,-1.03213203435478,11.1));
#38574=CARTESIAN_POINT('',(-2.,-1.15,7.3));
#38575=CARTESIAN_POINT('',(2.,0.167867965645222,11.1));
#38576=CARTESIAN_POINT('',(-2.,0.05,7.3));
#38577=CARTESIAN_POINT('',(0.,-0.25,7.3));
#38578=CARTESIAN_POINT('',(0.,-0.65,7.3));
#38579=CARTESIAN_POINT('',(-1.51,0.,3.4));
#38580=UNCERTAINTY_MEASURE_WITH_UNIT(LENGTH_MEASURE(0.001),#38612,
'DISTANCE_ACCURACY_VALUE',
'Maximum model space distance between geometric entities at asserted c
onnectivities');
#38581=UNCERTAINTY_MEASURE_WITH_UNIT(LENGTH_MEASURE(0.001),#38612,
'DISTANCE_ACCURACY_VALUE',
'Maximum model space distance between geometric entities at asserted c
onnectivities');
#38582=UNCERTAINTY_MEASURE_WITH_UNIT(LENGTH_MEASURE(0.001),#38612,
'DISTANCE_ACCURACY_VALUE',
'Maximum model space distance between geometric entities at asserted c
onnectivities');
#38583=UNCERTAINTY_MEASURE_WITH_UNIT(LENGTH_MEASURE(0.001),#38612,
'DISTANCE_ACCURACY_VALUE',
'Maximum model space distance between geometric entities at asserted c
onnectivities');
#38584=UNCERTAINTY_MEASURE_WITH_UNIT(LENGTH_MEASURE(0.001),#38612,
'DISTANCE_ACCURACY_VALUE',
'Maximum model space distance between geometric entities at asserted c
onnectivities');
#38585=UNCERTAINTY_MEASURE_WITH_UNIT(LENGTH_MEASURE(0.001),#38612,
'DISTANCE_ACCURACY_VALUE',
'Maximum model space distance between geometric entities at asserted c
onnectivities');
#38586=UNCERTAINTY_MEASURE_WITH_UNIT(LENGTH_MEASURE(0.001),#38612,
'DISTANCE_ACCURACY_VALUE',
'Maximum model space distance between geometric entities at asserted c
onnectivities');
#38587=UNCERTAINTY_MEASURE_WITH_UNIT(LENGTH_MEASURE(0.001),#38612,
'DISTANCE_ACCURACY_VALUE',
'Maximum model space distance between geometric entities at asserted c
onnectivities');
#38588=UNCERTAINTY_MEASURE_WITH_UNIT(LENGTH_MEASURE(0.001),#38612,
'DISTANCE_ACCURACY_VALUE',
'Maximum model space distance between geometric entities at asserted c
onnectivities');
#38589=UNCERTAINTY_MEASURE_WITH_UNIT(LENGTH_MEASURE(0.001),#38612,
'DISTANCE_ACCURACY_VALUE',
'Maximum model space distance between geometric entities at asserted c
onnectivities');
#38590=UNCERTAINTY_MEASURE_WITH_UNIT(LENGTH_MEASURE(0.001),#38612,
'DISTANCE_ACCURACY_VALUE',
'Maximum model space distance between geometric entities at asserted c
onnectivities');
#38591=UNCERTAINTY_MEASURE_WITH_UNIT(LENGTH_MEASURE(0.001),#38612,
'DISTANCE_ACCURACY_VALUE',
'Maximum model space distance between geometric entities at asserted c
onnectivities');
#38592=UNCERTAINTY_MEASURE_WITH_UNIT(LENGTH_MEASURE(0.001),#38612,
'DISTANCE_ACCURACY_VALUE',
'Maximum model space distance between geometric entities at asserted c
onnectivities');
#38593=UNCERTAINTY_MEASURE_WITH_UNIT(LENGTH_MEASURE(0.001),#38612,
'DISTANCE_ACCURACY_VALUE',
'Maximum model space distance between geometric entities at asserted c
onnectivities');
#38594=UNCERTAINTY_MEASURE_WITH_UNIT(LENGTH_MEASURE(0.001),#38612,
'DISTANCE_ACCURACY_VALUE',
'Maximum model space distance between geometric entities at asserted c
onnectivities');
#38595=UNCERTAINTY_MEASURE_WITH_UNIT(LENGTH_MEASURE(0.001),#38612,
'DISTANCE_ACCURACY_VALUE',
'Maximum model space distance between geometric entities at asserted c
onnectivities');
#38596=(
GEOMETRIC_REPRESENTATION_CONTEXT(3)
GLOBAL_UNCERTAINTY_ASSIGNED_CONTEXT((#38580))
GLOBAL_UNIT_ASSIGNED_CONTEXT((#38612,#38614,#38615))
REPRESENTATION_CONTEXT('','3D')
);
#38597=(
GEOMETRIC_REPRESENTATION_CONTEXT(3)
GLOBAL_UNCERTAINTY_ASSIGNED_CONTEXT((#38581))
GLOBAL_UNIT_ASSIGNED_CONTEXT((#38612,#38614,#38615))
REPRESENTATION_CONTEXT('','3D')
);
#38598=(
GEOMETRIC_REPRESENTATION_CONTEXT(3)
GLOBAL_UNCERTAINTY_ASSIGNED_CONTEXT((#38582))
GLOBAL_UNIT_ASSIGNED_CONTEXT((#38612,#38614,#38615))
REPRESENTATION_CONTEXT('','3D')
);
#38599=(
GEOMETRIC_REPRESENTATION_CONTEXT(3)
GLOBAL_UNCERTAINTY_ASSIGNED_CONTEXT((#38583))
GLOBAL_UNIT_ASSIGNED_CONTEXT((#38612,#38614,#38615))
REPRESENTATION_CONTEXT('','3D')
);
#38600=(
GEOMETRIC_REPRESENTATION_CONTEXT(3)
GLOBAL_UNCERTAINTY_ASSIGNED_CONTEXT((#38584))
GLOBAL_UNIT_ASSIGNED_CONTEXT((#38612,#38614,#38615))
REPRESENTATION_CONTEXT('','3D')
);
#38601=(
GEOMETRIC_REPRESENTATION_CONTEXT(3)
GLOBAL_UNCERTAINTY_ASSIGNED_CONTEXT((#38585))
GLOBAL_UNIT_ASSIGNED_CONTEXT((#38612,#38614,#38615))
REPRESENTATION_CONTEXT('','3D')
);
#38602=(
GEOMETRIC_REPRESENTATION_CONTEXT(3)
GLOBAL_UNCERTAINTY_ASSIGNED_CONTEXT((#38586))
GLOBAL_UNIT_ASSIGNED_CONTEXT((#38612,#38614,#38615))
REPRESENTATION_CONTEXT('','3D')
);
#38603=(
GEOMETRIC_REPRESENTATION_CONTEXT(3)
GLOBAL_UNCERTAINTY_ASSIGNED_CONTEXT((#38587))
GLOBAL_UNIT_ASSIGNED_CONTEXT((#38612,#38614,#38615))
REPRESENTATION_CONTEXT('','3D')
);
#38604=(
GEOMETRIC_REPRESENTATION_CONTEXT(3)
GLOBAL_UNCERTAINTY_ASSIGNED_CONTEXT((#38588))
GLOBAL_UNIT_ASSIGNED_CONTEXT((#38612,#38614,#38615))
REPRESENTATION_CONTEXT('','3D')
);
#38605=(
GEOMETRIC_REPRESENTATION_CONTEXT(3)
GLOBAL_UNCERTAINTY_ASSIGNED_CONTEXT((#38589))
GLOBAL_UNIT_ASSIGNED_CONTEXT((#38612,#38614,#38615))
REPRESENTATION_CONTEXT('','3D')
);
#38606=(
GEOMETRIC_REPRESENTATION_CONTEXT(3)
GLOBAL_UNCERTAINTY_ASSIGNED_CONTEXT((#38590))
GLOBAL_UNIT_ASSIGNED_CONTEXT((#38612,#38614,#38615))
REPRESENTATION_CONTEXT('','3D')
);
#38607=(
GEOMETRIC_REPRESENTATION_CONTEXT(3)
GLOBAL_UNCERTAINTY_ASSIGNED_CONTEXT((#38591))
GLOBAL_UNIT_ASSIGNED_CONTEXT((#38612,#38614,#38615))
REPRESENTATION_CONTEXT('','3D')
);
#38608=(
GEOMETRIC_REPRESENTATION_CONTEXT(3)
GLOBAL_UNCERTAINTY_ASSIGNED_CONTEXT((#38592))
GLOBAL_UNIT_ASSIGNED_CONTEXT((#38612,#38614,#38615))
REPRESENTATION_CONTEXT('','3D')
);
#38609=(
GEOMETRIC_REPRESENTATION_CONTEXT(3)
GLOBAL_UNCERTAINTY_ASSIGNED_CONTEXT((#38593))
GLOBAL_UNIT_ASSIGNED_CONTEXT((#38612,#38614,#38615))
REPRESENTATION_CONTEXT('','3D')
);
#38610=(
GEOMETRIC_REPRESENTATION_CONTEXT(3)
GLOBAL_UNCERTAINTY_ASSIGNED_CONTEXT((#38594))
GLOBAL_UNIT_ASSIGNED_CONTEXT((#38612,#38614,#38615))
REPRESENTATION_CONTEXT('','3D')
);
#38611=(
GEOMETRIC_REPRESENTATION_CONTEXT(3)
GLOBAL_UNCERTAINTY_ASSIGNED_CONTEXT((#38595))
GLOBAL_UNIT_ASSIGNED_CONTEXT((#38612,#38614,#38615))
REPRESENTATION_CONTEXT('','3D')
);
#38612=(
LENGTH_UNIT()
NAMED_UNIT(*)
SI_UNIT(.CENTI.,.METRE.)
);
#38613=(
LENGTH_UNIT()
NAMED_UNIT(*)
SI_UNIT($,.METRE.)
);
#38614=(
NAMED_UNIT(*)
PLANE_ANGLE_UNIT()
SI_UNIT($,.RADIAN.)
);
#38615=(
NAMED_UNIT(*)
SI_UNIT($,.STERADIAN.)
SOLID_ANGLE_UNIT()
);
#38616=SHAPE_DEFINITION_REPRESENTATION(#38631,#38667);
#38617=SHAPE_DEFINITION_REPRESENTATION(#38632,#38668);
#38618=SHAPE_DEFINITION_REPRESENTATION(#38633,#38669);
#38619=SHAPE_DEFINITION_REPRESENTATION(#38634,#38670);
#38620=SHAPE_DEFINITION_REPRESENTATION(#38635,#38671);
#38621=SHAPE_DEFINITION_REPRESENTATION(#38636,#38672);
#38622=SHAPE_DEFINITION_REPRESENTATION(#38637,#38673);
#38623=SHAPE_DEFINITION_REPRESENTATION(#38638,#38674);
#38624=SHAPE_DEFINITION_REPRESENTATION(#38639,#38675);
#38625=SHAPE_DEFINITION_REPRESENTATION(#38640,#38676);
#38626=SHAPE_DEFINITION_REPRESENTATION(#38641,#38677);
#38627=SHAPE_DEFINITION_REPRESENTATION(#38642,#38678);
#38628=SHAPE_DEFINITION_REPRESENTATION(#38643,#38679);
#38629=SHAPE_DEFINITION_REPRESENTATION(#38644,#38680);
#38630=SHAPE_DEFINITION_REPRESENTATION(#38645,#38681);
#38631=PRODUCT_DEFINITION_SHAPE('',$,#38683);
#38632=PRODUCT_DEFINITION_SHAPE('',$,#38684);
#38633=PRODUCT_DEFINITION_SHAPE('',$,#38685);
#38634=PRODUCT_DEFINITION_SHAPE('',$,#38686);
#38635=PRODUCT_DEFINITION_SHAPE('',$,#38687);
#38636=PRODUCT_DEFINITION_SHAPE('',$,#38688);
#38637=PRODUCT_DEFINITION_SHAPE('',$,#38689);
#38638=PRODUCT_DEFINITION_SHAPE('',$,#38690);
#38639=PRODUCT_DEFINITION_SHAPE('',$,#38691);
#38640=PRODUCT_DEFINITION_SHAPE('',$,#38692);
#38641=PRODUCT_DEFINITION_SHAPE('',$,#38693);
#38642=PRODUCT_DEFINITION_SHAPE('',$,#38694);
#38643=PRODUCT_DEFINITION_SHAPE('',$,#38695);
#38644=PRODUCT_DEFINITION_SHAPE('',$,#38696);
#38645=PRODUCT_DEFINITION_SHAPE('',$,#38697);
#38646=PRODUCT_DEFINITION_SHAPE($,$,#74);
#38647=PRODUCT_DEFINITION_SHAPE($,$,#75);
#38648=PRODUCT_DEFINITION_SHAPE($,$,#76);
#38649=PRODUCT_DEFINITION_SHAPE($,$,#77);
#38650=PRODUCT_DEFINITION_SHAPE($,$,#78);
#38651=PRODUCT_DEFINITION_SHAPE($,$,#79);
#38652=PRODUCT_DEFINITION_SHAPE($,$,#80);
#38653=PRODUCT_DEFINITION_SHAPE($,$,#81);
#38654=PRODUCT_DEFINITION_SHAPE($,$,#82);
#38655=PRODUCT_DEFINITION_SHAPE($,$,#83);
#38656=PRODUCT_DEFINITION_SHAPE($,$,#84);
#38657=PRODUCT_DEFINITION_SHAPE($,$,#85);
#38658=PRODUCT_DEFINITION_SHAPE($,$,#86);
#38659=PRODUCT_DEFINITION_SHAPE($,$,#87);
#38660=PRODUCT_DEFINITION_SHAPE($,$,#88);
#38661=PRODUCT_DEFINITION_SHAPE($,$,#89);
#38662=PRODUCT_DEFINITION_SHAPE($,$,#90);
#38663=PRODUCT_DEFINITION_SHAPE($,$,#91);
#38664=PRODUCT_DEFINITION_SHAPE($,$,#92);
#38665=PRODUCT_DEFINITION_SHAPE($,$,#93);
#38666=PRODUCT_DEFINITION_SHAPE($,$,#94);
#38667=SHAPE_REPRESENTATION('',(#16403,#17784,#17785,#17786,#17787,#17788,
#17789,#17790,#17791,#17792,#17793,#17794,#17795,#17796,#17797,#17798,#17799,
#17800,#17801,#17802,#17803,#17804),#38596);
#38668=SHAPE_REPRESENTATION('',(#16404),#38597);
#38669=SHAPE_REPRESENTATION('',(#16581),#38598);
#38670=SHAPE_REPRESENTATION('',(#16625),#38599);
#38671=SHAPE_REPRESENTATION('',(#16649),#38600);
#38672=SHAPE_REPRESENTATION('',(#16774),#38601);
#38673=SHAPE_REPRESENTATION('',(#16784),#38602);
#38674=SHAPE_REPRESENTATION('',(#16834),#38603);
#38675=SHAPE_REPRESENTATION('',(#16909),#38604);
#38676=SHAPE_REPRESENTATION('',(#16983),#38605);
#38677=SHAPE_REPRESENTATION('',(#17098),#38606);
#38678=SHAPE_REPRESENTATION('',(#17324),#38607);
#38679=SHAPE_REPRESENTATION('',(#17327),#38608);
#38680=SHAPE_REPRESENTATION('',(#17332),#38609);
#38681=SHAPE_REPRESENTATION('',(#17623),#38610);
#38682=PRODUCT_DEFINITION_CONTEXT('part definition',#38729,'design');
#38683=PRODUCT_DEFINITION('2026-10-19-02-27-11-155','MAS-303',#38698,#38682);
#38684=PRODUCT_DEFINITION('2026-10-19-02-31-24-157',
'01_Slotted_Foot_Base_with_Post_Socket_80x60',#38699,#38682);
#38685=PRODUCT_DEFINITION('2026-10-19-02-31-27-829',
'02_Outer_Post_Tube_D20_with_Lock_Collar',#38700,#38682);
#38686=PRODUCT_DEFINITION('2026-10-19-02-31-28-533',
'03_Inner_Height_Adjust_Rod_D14',#38701,#38682);
#38687=PRODUCT_DEFINITION('2026-10-19-02-31-31-424',
'05_Adjustable_Mirror_Plate_56x56',#38702,#38682);
#38688=PRODUCT_DEFINITION('2026-10-19-02-31-35-057',
'06_HR_Laser_Cavity_Mirror_Si_Au_D25x3',#38703,#38682);
#38689=PRODUCT_DEFINITION('2026-10-19-02-31-35-672',
'07_Mirror_Retaining_Thread_Bezel_M27x1',#38704,#38682);
#38690=PRODUCT_DEFINITION('2026-10-19-02-32-11-430',
'13_ISO_4026_M4x5_Set_Screw',#38705,#38682);
#38691=PRODUCT_DEFINITION('2026-10-19-02-32-13-450',
'14_ISO_4026_M4x4_Set_Screw',#38706,#38682);
#38692=PRODUCT_DEFINITION('2026-10-19-02-32-41-507',
'04_Fixed_L-Bracket_Kinematic_Back_Plate',#38707,#38682);
#38693=PRODUCT_DEFINITION('2026-10-19-02-31-37-420',
'08_Brass_Knurled_Fine_Adjust_Screw_M5x0.5x12',#38708,#38682);
#38694=PRODUCT_DEFINITION('2026-10-19-02-31-51-310',
'09_DIN_5401_Steel_Ball_D3_G25',#38709,#38682);
#38695=PRODUCT_DEFINITION('2026-10-19-02-31-51-889',
'10_Preload_Compression_Spring_D7.2x0.6x4',#38710,#38682);
#38696=PRODUCT_DEFINITION('2026-10-19-02-31-53-467',
'11_ISO_4762_M4x16_Preload_Screw',#38711,#38682);
#38697=PRODUCT_DEFINITION('2026-10-19-02-32-05-072',
'12_Brass_Knurled_Thumb_Lock_Screw_M4x8',#38712,#38682);
#38698=PRODUCT_DEFINITION_FORMATION('',$,#38731);
#38699=PRODUCT_DEFINITION_FORMATION('',$,#38732);
#38700=PRODUCT_DEFINITION_FORMATION('',$,#38733);
#38701=PRODUCT_DEFINITION_FORMATION('',$,#38734);
#38702=PRODUCT_DEFINITION_FORMATION('',$,#38735);
#38703=PRODUCT_DEFINITION_FORMATION('',$,#38736);
#38704=PRODUCT_DEFINITION_FORMATION('',$,#38737);
#38705=PRODUCT_DEFINITION_FORMATION('',$,#38738);
#38706=PRODUCT_DEFINITION_FORMATION('',$,#38739);
#38707=PRODUCT_DEFINITION_FORMATION('',$,#38740);
#38708=PRODUCT_DEFINITION_FORMATION('',$,#38741);
#38709=PRODUCT_DEFINITION_FORMATION('',$,#38742);
#38710=PRODUCT_DEFINITION_FORMATION('',$,#38743);
#38711=PRODUCT_DEFINITION_FORMATION('',$,#38744);
#38712=PRODUCT_DEFINITION_FORMATION('',$,#38745);
#38713=PRODUCT_RELATED_PRODUCT_CATEGORY('MAS-303','MAS-303',(#38731));
#38714=PRODUCT_RELATED_PRODUCT_CATEGORY(
'01_Slotted_Foot_Base_with_Post_Socket_80x60',
'01_Slotted_Foot_Base_with_Post_Socket_80x60',(#38732));
#38715=PRODUCT_RELATED_PRODUCT_CATEGORY(
'02_Outer_Post_Tube_D20_with_Lock_Collar',
'02_Outer_Post_Tube_D20_with_Lock_Collar',(#38733));
#38716=PRODUCT_RELATED_PRODUCT_CATEGORY(
'03_Inner_Height_Adjust_Rod_D14','03_Inner_Height_Adjust_Rod_D14',(#38734));
#38717=PRODUCT_RELATED_PRODUCT_CATEGORY(
'05_Adjustable_Mirror_Plate_56x56','05_Adjustable_Mirror_Plate_56x56',(#38735));
#38718=PRODUCT_RELATED_PRODUCT_CATEGORY(
'06_HR_Laser_Cavity_Mirror_Si_Au_D25x3',
'06_HR_Laser_Cavity_Mirror_Si_Au_D25x3',(#38736));
#38719=PRODUCT_RELATED_PRODUCT_CATEGORY(
'07_Mirror_Retaining_Thread_Bezel_M27x1',
'07_Mirror_Retaining_Thread_Bezel_M27x1',(#38737));
#38720=PRODUCT_RELATED_PRODUCT_CATEGORY('13_ISO_4026_M4x5_Set_Screw',
'13_ISO_4026_M4x5_Set_Screw',(#38738));
#38721=PRODUCT_RELATED_PRODUCT_CATEGORY('14_ISO_4026_M4x4_Set_Screw',
'14_ISO_4026_M4x4_Set_Screw',(#38739));
#38722=PRODUCT_RELATED_PRODUCT_CATEGORY(
'04_Fixed_L-Bracket_Kinematic_Back_Plate',
'04_Fixed_L-Bracket_Kinematic_Back_Plate',(#38740));
#38723=PRODUCT_RELATED_PRODUCT_CATEGORY(
'08_Brass_Knurled_Fine_Adjust_Screw_M5x0.5x12',
'08_Brass_Knurled_Fine_Adjust_Screw_M5x0.5x12',(#38741));
#38724=PRODUCT_RELATED_PRODUCT_CATEGORY('09_DIN_5401_Steel_Ball_D3_G25',
'09_DIN_5401_Steel_Ball_D3_G25',(#38742));
#38725=PRODUCT_RELATED_PRODUCT_CATEGORY(
'10_Preload_Compression_Spring_D7.2x0.6x4',
'10_Preload_Compression_Spring_D7.2x0.6x4',(#38743));
#38726=PRODUCT_RELATED_PRODUCT_CATEGORY(
'11_ISO_4762_M4x16_Preload_Screw','11_ISO_4762_M4x16_Preload_Screw',(#38744));
#38727=PRODUCT_RELATED_PRODUCT_CATEGORY(
'12_Brass_Knurled_Thumb_Lock_Screw_M4x8',
'12_Brass_Knurled_Thumb_Lock_Screw_M4x8',(#38745));
#38728=APPLICATION_PROTOCOL_DEFINITION('international standard',
'automotive_design',2009,#38729);
#38729=APPLICATION_CONTEXT(
'Core Data for Automotive Mechanical Design Process');
#38730=PRODUCT_CONTEXT('part definition',#38729,'mechanical');
#38731=PRODUCT('2026-10-19-02-27-11-155','MAS-303',$,(#38730));
#38732=PRODUCT('2026-10-19-02-31-24-157',
'01_Slotted_Foot_Base_with_Post_Socket_80x60',$,(#38730));
#38733=PRODUCT('2026-10-19-02-31-27-829',
'02_Outer_Post_Tube_D20_with_Lock_Collar',$,(#38730));
#38734=PRODUCT('2026-10-19-02-31-28-533',
'03_Inner_Height_Adjust_Rod_D14',$,(#38730));
#38735=PRODUCT('2026-10-19-02-31-31-424',
'05_Adjustable_Mirror_Plate_56x56',$,(#38730));
#38736=PRODUCT('2026-10-19-02-31-35-057',
'06_HR_Laser_Cavity_Mirror_Si_Au_D25x3',$,(#38730));
#38737=PRODUCT('2026-10-19-02-31-35-672',
'07_Mirror_Retaining_Thread_Bezel_M27x1',$,(#38730));
#38738=PRODUCT('2026-10-19-02-32-11-430','13_ISO_4026_M4x5_Set_Screw',$,
(#38730));
#38739=PRODUCT('2026-10-19-02-32-13-450','14_ISO_4026_M4x4_Set_Screw',$,
(#38730));
#38740=PRODUCT('2026-10-19-02-32-41-507',
'04_Fixed_L-Bracket_Kinematic_Back_Plate',$,(#38730));
#38741=PRODUCT('2026-10-19-02-31-37-420',
'08_Brass_Knurled_Fine_Adjust_Screw_M5x0.5x12',$,(#38730));
#38742=PRODUCT('2026-10-19-02-31-51-310',
'09_DIN_5401_Steel_Ball_D3_G25',$,(#38730));
#38743=PRODUCT('2026-10-19-02-31-51-889',
'10_Preload_Compression_Spring_D7.2x0.6x4',$,(#38730));
#38744=PRODUCT('2026-10-19-02-31-53-467',
'11_ISO_4762_M4x16_Preload_Screw',$,(#38730));
#38745=PRODUCT('2026-10-19-02-32-05-072',
'12_Brass_Knurled_Thumb_Lock_Screw_M4x8',$,(#38730));
#38746=PRESENTATION_STYLE_ASSIGNMENT((#38761));
#38747=PRESENTATION_STYLE_ASSIGNMENT((#38762));
#38748=PRESENTATION_STYLE_ASSIGNMENT((#38763));
#38749=PRESENTATION_STYLE_ASSIGNMENT((#38764));
#38750=PRESENTATION_STYLE_ASSIGNMENT((#38765));
#38751=PRESENTATION_STYLE_ASSIGNMENT((#38766));
#38752=PRESENTATION_STYLE_ASSIGNMENT((#38767));
#38753=PRESENTATION_STYLE_ASSIGNMENT((#38768));
#38754=PRESENTATION_STYLE_ASSIGNMENT((#38769));
#38755=PRESENTATION_STYLE_ASSIGNMENT((#38770));
#38756=PRESENTATION_STYLE_ASSIGNMENT((#38771));
#38757=PRESENTATION_STYLE_ASSIGNMENT((#38772));
#38758=PRESENTATION_STYLE_ASSIGNMENT((#38773));
#38759=PRESENTATION_STYLE_ASSIGNMENT((#38774));
#38760=PRESENTATION_STYLE_ASSIGNMENT((#38775));
#38761=SURFACE_STYLE_USAGE(.BOTH.,#38776);
#38762=SURFACE_STYLE_USAGE(.BOTH.,#38777);
#38763=SURFACE_STYLE_USAGE(.BOTH.,#38778);
#38764=SURFACE_STYLE_USAGE(.BOTH.,#38779);
#38765=SURFACE_STYLE_USAGE(.BOTH.,#38780);
#38766=SURFACE_STYLE_USAGE(.BOTH.,#38781);
#38767=SURFACE_STYLE_USAGE(.BOTH.,#38782);
#38768=SURFACE_STYLE_USAGE(.BOTH.,#38783);
#38769=SURFACE_STYLE_USAGE(.BOTH.,#38784);
#38770=SURFACE_STYLE_USAGE(.BOTH.,#38785);
#38771=SURFACE_STYLE_USAGE(.BOTH.,#38786);
#38772=SURFACE_STYLE_USAGE(.BOTH.,#38787);
#38773=SURFACE_STYLE_USAGE(.BOTH.,#38788);
#38774=SURFACE_STYLE_USAGE(.BOTH.,#38789);
#38775=SURFACE_STYLE_USAGE(.BOTH.,#38790);
#38776=SURFACE_SIDE_STYLE('',(#38791));
#38777=SURFACE_SIDE_STYLE('',(#38792));
#38778=SURFACE_SIDE_STYLE('',(#38793));
#38779=SURFACE_SIDE_STYLE('',(#38794));
#38780=SURFACE_SIDE_STYLE('',(#38795));
#38781=SURFACE_SIDE_STYLE('',(#38796));
#38782=SURFACE_SIDE_STYLE('',(#38797));
#38783=SURFACE_SIDE_STYLE('',(#38798));
#38784=SURFACE_SIDE_STYLE('',(#38799));
#38785=SURFACE_SIDE_STYLE('',(#38800));
#38786=SURFACE_SIDE_STYLE('',(#38801));
#38787=SURFACE_SIDE_STYLE('',(#38802));
#38788=SURFACE_SIDE_STYLE('',(#38803));
#38789=SURFACE_SIDE_STYLE('',(#38804));
#38790=SURFACE_SIDE_STYLE('',(#38805));
#38791=SURFACE_STYLE_FILL_AREA(#38806);
#38792=SURFACE_STYLE_FILL_AREA(#38807);
#38793=SURFACE_STYLE_FILL_AREA(#38808);
#38794=SURFACE_STYLE_FILL_AREA(#38809);
#38795=SURFACE_STYLE_FILL_AREA(#38810);
#38796=SURFACE_STYLE_FILL_AREA(#38811);
#38797=SURFACE_STYLE_FILL_AREA(#38812);
#38798=SURFACE_STYLE_FILL_AREA(#38813);
#38799=SURFACE_STYLE_FILL_AREA(#38814);
#38800=SURFACE_STYLE_FILL_AREA(#38815);
#38801=SURFACE_STYLE_FILL_AREA(#38816);
#38802=SURFACE_STYLE_FILL_AREA(#38817);
#38803=SURFACE_STYLE_FILL_AREA(#38818);
#38804=SURFACE_STYLE_FILL_AREA(#38819);
#38805=SURFACE_STYLE_FILL_AREA(#38820);
#38806=FILL_AREA_STYLE('Steel - Satin',(#38821));
#38807=FILL_AREA_STYLE('MAS303_foot',(#38822));
#38808=FILL_AREA_STYLE('MAS303_tube',(#38823));
#38809=FILL_AREA_STYLE('MAS303_rod',(#38824));
#38810=FILL_AREA_STYLE('MAS303_fp',(#38825));
#38811=FILL_AREA_STYLE('MAS303_mir',(#38826));
#38812=FILL_AREA_STYLE('MAS303_ring',(#38827));
#38813=FILL_AREA_STYLE('MAS303_set5',(#38828));
#38814=FILL_AREA_STYLE('MAS303_set4',(#38829));
#38815=FILL_AREA_STYLE('MAS303_brk',(#38830));
#38816=FILL_AREA_STYLE('MAS303_adj',(#38831));
#38817=FILL_AREA_STYLE('MAS303_ball',(#38832));
#38818=FILL_AREA_STYLE('MAS303_spr',(#38833));
#38819=FILL_AREA_STYLE('MAS303_shc',(#38834));
#38820=FILL_AREA_STYLE('MAS303_thumb',(#38835));
#38821=FILL_AREA_STYLE_COLOUR('Steel - Satin',#38836);
#38822=FILL_AREA_STYLE_COLOUR('MAS303_foot',#38837);
#38823=FILL_AREA_STYLE_COLOUR('MAS303_tube',#38838);
#38824=FILL_AREA_STYLE_COLOUR('MAS303_rod',#38839);
#38825=FILL_AREA_STYLE_COLOUR('MAS303_fp',#38840);
#38826=FILL_AREA_STYLE_COLOUR('MAS303_mir',#38841);
#38827=FILL_AREA_STYLE_COLOUR('MAS303_ring',#38842);
#38828=FILL_AREA_STYLE_COLOUR('MAS303_set5',#38843);
#38829=FILL_AREA_STYLE_COLOUR('MAS303_set4',#38844);
#38830=FILL_AREA_STYLE_COLOUR('MAS303_brk',#38845);
#38831=FILL_AREA_STYLE_COLOUR('MAS303_adj',#38846);
#38832=FILL_AREA_STYLE_COLOUR('MAS303_ball',#38847);
#38833=FILL_AREA_STYLE_COLOUR('MAS303_spr',#38848);
#38834=FILL_AREA_STYLE_COLOUR('MAS303_shc',#38849);
#38835=FILL_AREA_STYLE_COLOUR('MAS303_thumb',#38850);
#38836=COLOUR_RGB('Steel - Satin',0.627450980392157,0.627450980392157,0.627450980392157);
#38837=COLOUR_RGB('MAS303_foot',0.109803921568627,0.109803921568627,0.117647058823529);
#38838=COLOUR_RGB('MAS303_tube',0.125490196078431,0.125490196078431,0.133333333333333);
#38839=COLOUR_RGB('MAS303_rod',0.141176470588235,0.141176470588235,0.149019607843137);
#38840=COLOUR_RGB('MAS303_fp',0.0980392156862745,0.0980392156862745,0.105882352941176);
#38841=COLOUR_RGB('MAS303_mir',0.886274509803922,0.752941176470588,0.470588235294118);
#38842=COLOUR_RGB('MAS303_ring',0.156862745098039,0.156862745098039,0.164705882352941);
#38843=COLOUR_RGB('MAS303_set5',0.776470588235294,0.792156862745098,0.815686274509804);
#38844=COLOUR_RGB('MAS303_set4',0.788235294117647,0.803921568627451,0.823529411764706);
#38845=COLOUR_RGB('MAS303_brk',0.117647058823529,0.117647058823529,0.125490196078431);
#38846=COLOUR_RGB('MAS303_adj',0.83921568627451,0.698039215686274,0.4);
#38847=COLOUR_RGB('MAS303_ball',0.847058823529412,0.858823529411765,0.87843137254902);
#38848=COLOUR_RGB('MAS303_spr',0.823529411764706,0.835294117647059,0.854901960784314);
#38849=COLOUR_RGB('MAS303_shc',0.784313725490196,0.8,0.819607843137255);
#38850=COLOUR_RGB('MAS303_thumb',0.831372549019608,0.690196078431373,0.392156862745098);
#38851=COLOUR_RGB('Dark Blue',0.08,0.2,0.34);
#38852=FILL_AREA_STYLE_COLOUR('',#38851);
#38853=FILL_AREA_STYLE('',(#38852));
#38854=SURFACE_STYLE_FILL_AREA(#38853);
#38855=SURFACE_SIDE_STYLE('',(#38854));
#38856=SURFACE_STYLE_USAGE(.BOTH.,#38855);
#38857=PRESENTATION_STYLE_ASSIGNMENT((#38856));
#38858=COLOUR_RGB('Light Blue',0.38,0.62,0.78);
#38859=FILL_AREA_STYLE_COLOUR('',#38858);
#38860=FILL_AREA_STYLE('',(#38859));
#38861=SURFACE_STYLE_FILL_AREA(#38860);
#38862=SURFACE_SIDE_STYLE('',(#38861));
#38863=SURFACE_STYLE_USAGE(.BOTH.,#38862);
#38864=PRESENTATION_STYLE_ASSIGNMENT((#38863));
#38865=COLOUR_RGB('Sky Blue',0.24,0.69,0.87);
#38866=FILL_AREA_STYLE_COLOUR('',#38865);
#38867=FILL_AREA_STYLE('',(#38866));
#38868=SURFACE_STYLE_FILL_AREA(#38867);
#38869=SURFACE_SIDE_STYLE('',(#38868));
#38870=SURFACE_STYLE_USAGE(.BOTH.,#38869);
#38871=PRESENTATION_STYLE_ASSIGNMENT((#38870));
#38872=COLOUR_RGB('Grey',0.48,0.52,0.57);
#38873=FILL_AREA_STYLE_COLOUR('',#38872);
#38874=FILL_AREA_STYLE('',(#38873));
#38875=SURFACE_STYLE_FILL_AREA(#38874);
#38876=SURFACE_SIDE_STYLE('',(#38875));
#38877=SURFACE_STYLE_USAGE(.BOTH.,#38876);
#38878=PRESENTATION_STYLE_ASSIGNMENT((#38877));
#38879=COLOUR_RGB('Black',0.12,0.14,0.17);
#38880=FILL_AREA_STYLE_COLOUR('',#38879);
#38881=FILL_AREA_STYLE('',(#38880));
#38882=SURFACE_STYLE_FILL_AREA(#38881);
#38883=SURFACE_SIDE_STYLE('',(#38882));
#38884=SURFACE_STYLE_USAGE(.BOTH.,#38883);
#38885=PRESENTATION_STYLE_ASSIGNMENT((#38884));
#38886=COLOUR_RGB('Off White',0.89,0.88,0.83);
#38887=FILL_AREA_STYLE_COLOUR('',#38886);
#38888=FILL_AREA_STYLE('',(#38887));
#38889=SURFACE_STYLE_FILL_AREA(#38888);
#38890=SURFACE_SIDE_STYLE('',(#38889));
#38891=SURFACE_STYLE_USAGE(.BOTH.,#38890);
#38892=PRESENTATION_STYLE_ASSIGNMENT((#38891));
ENDSEC;
END-ISO-10303-21;
